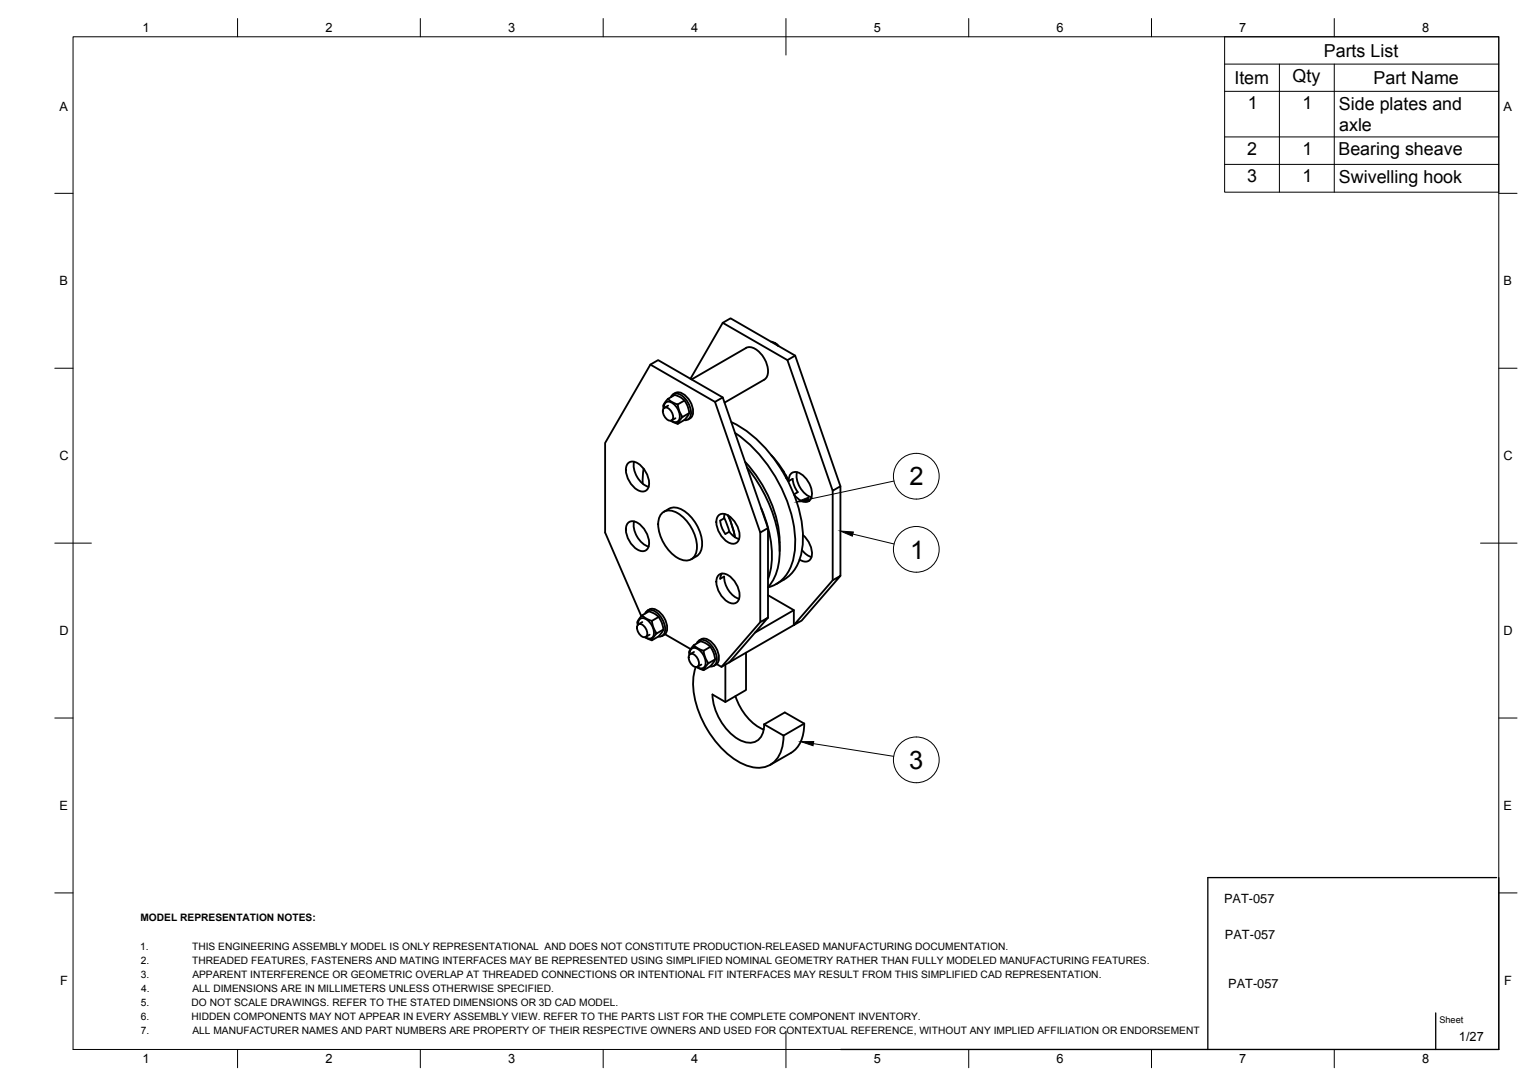
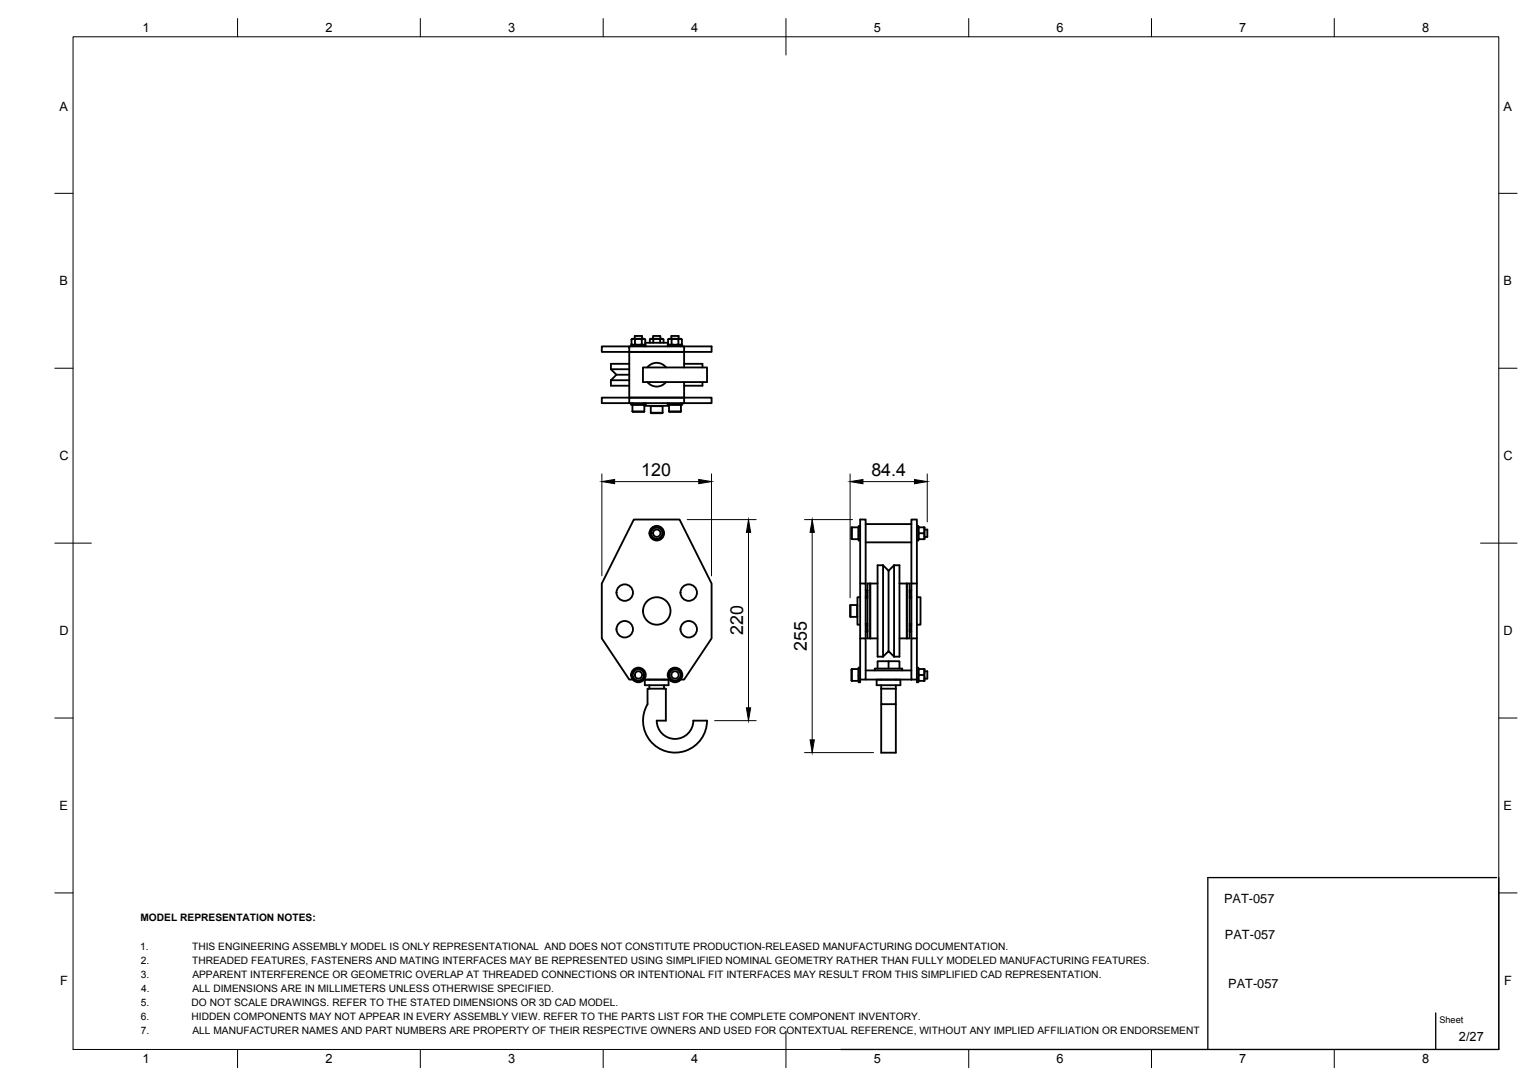
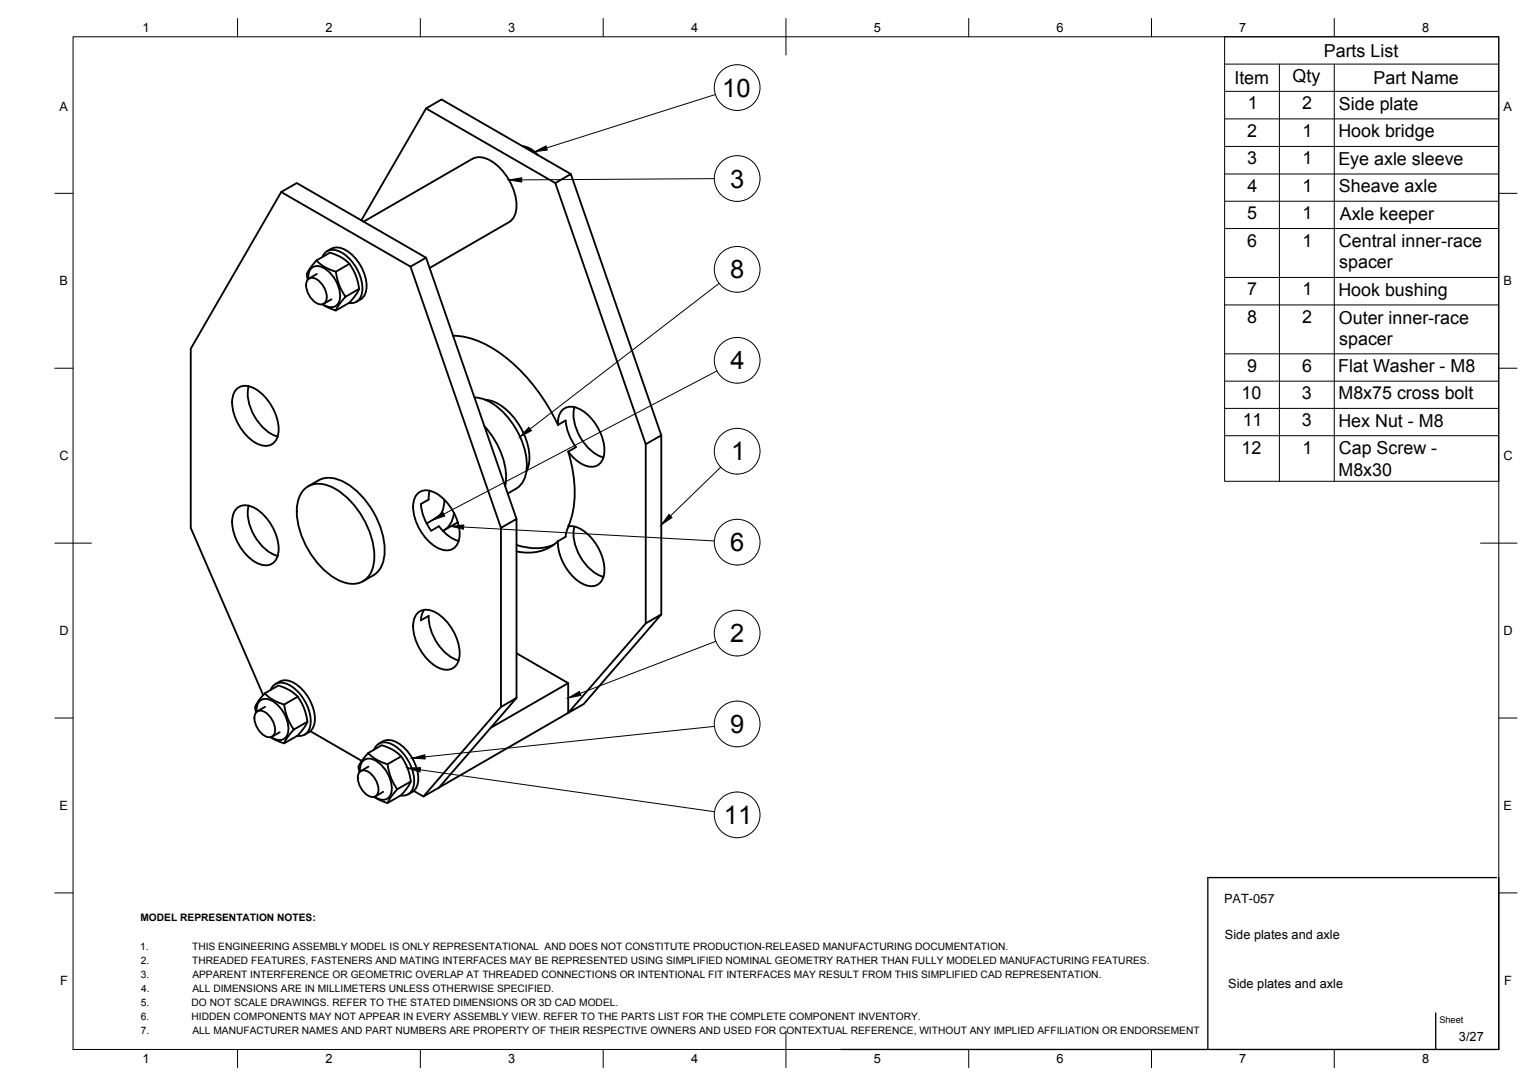
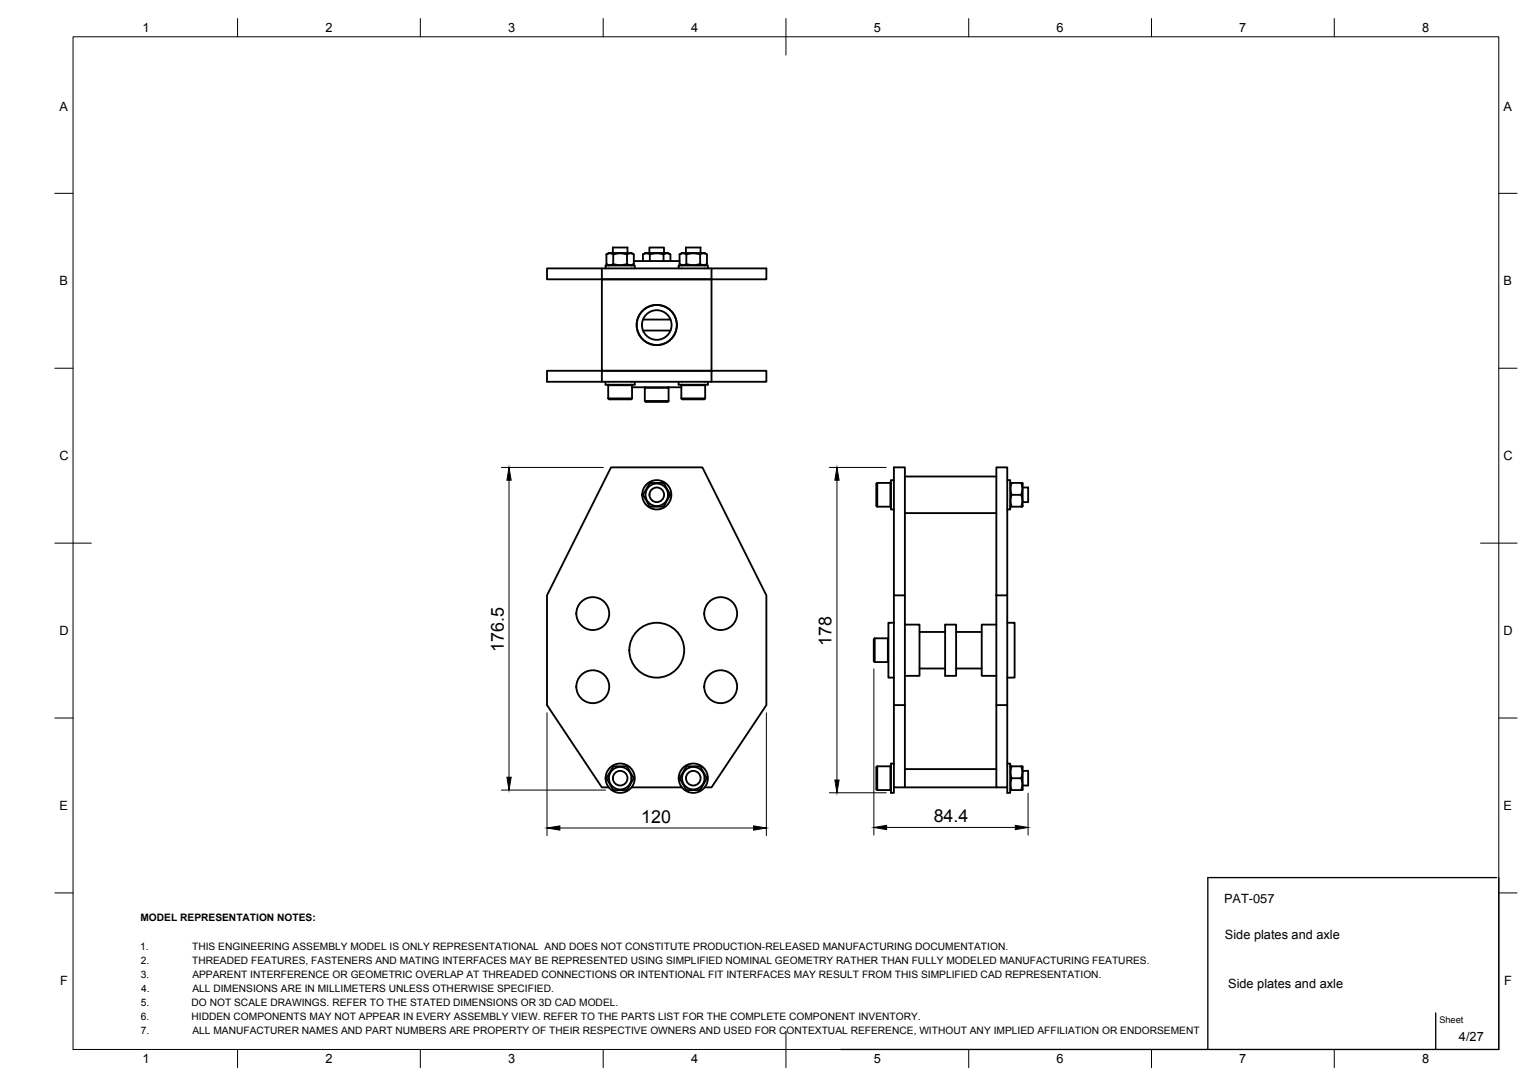
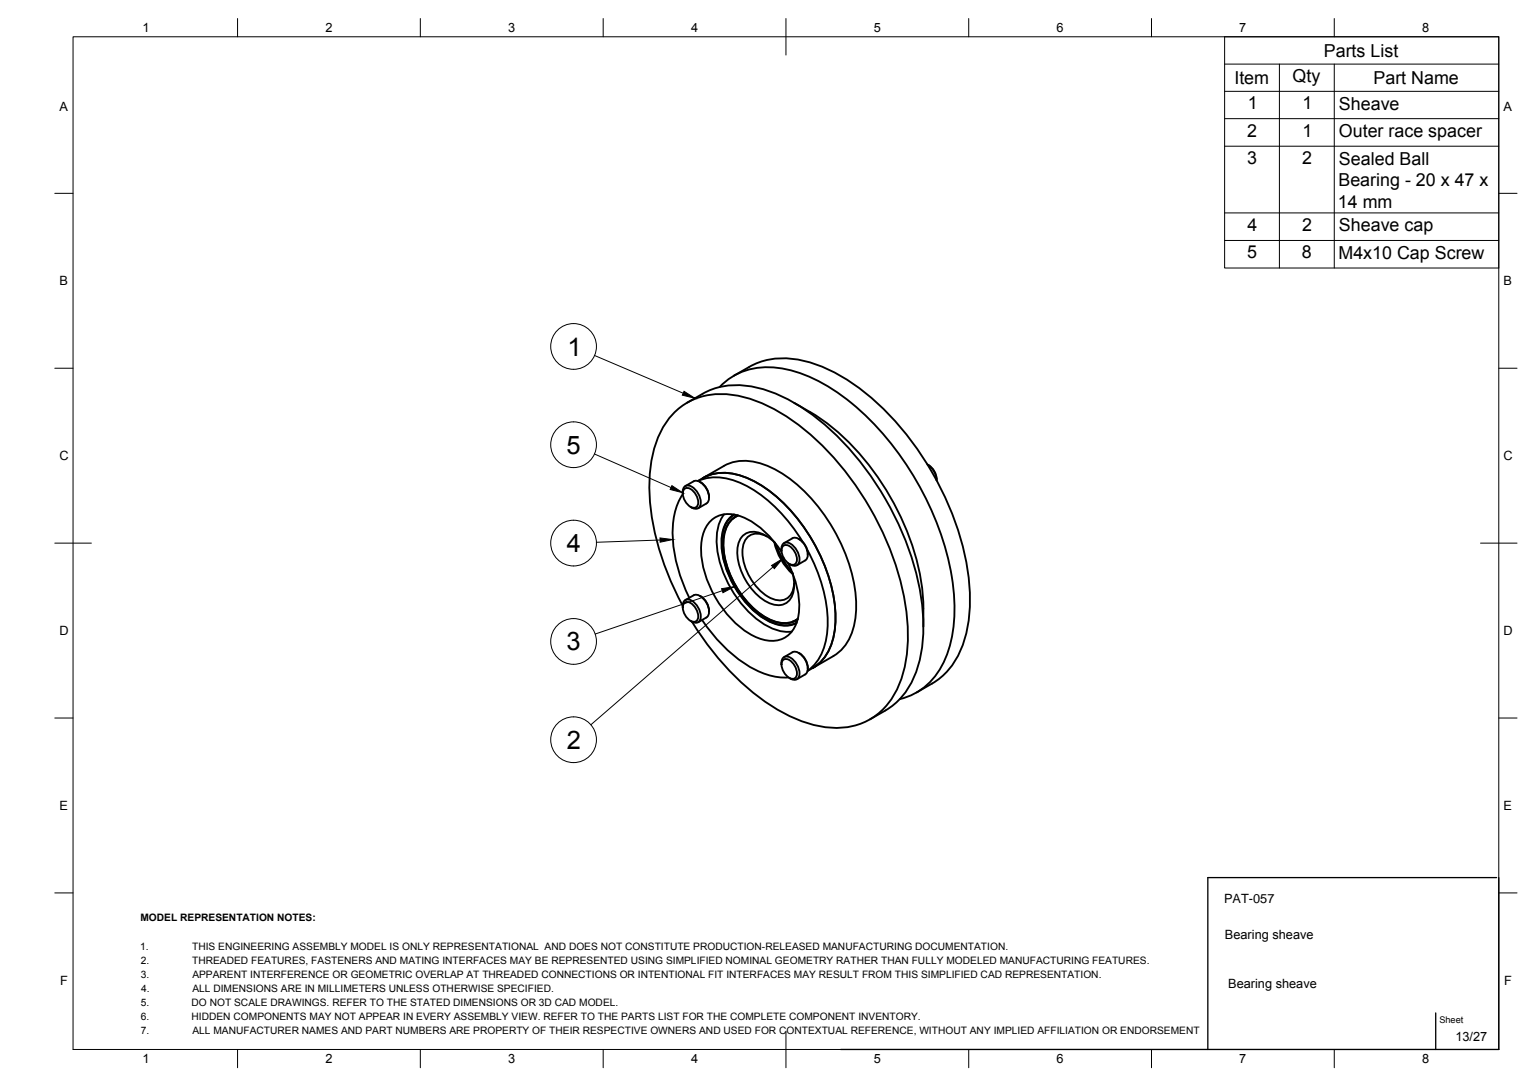
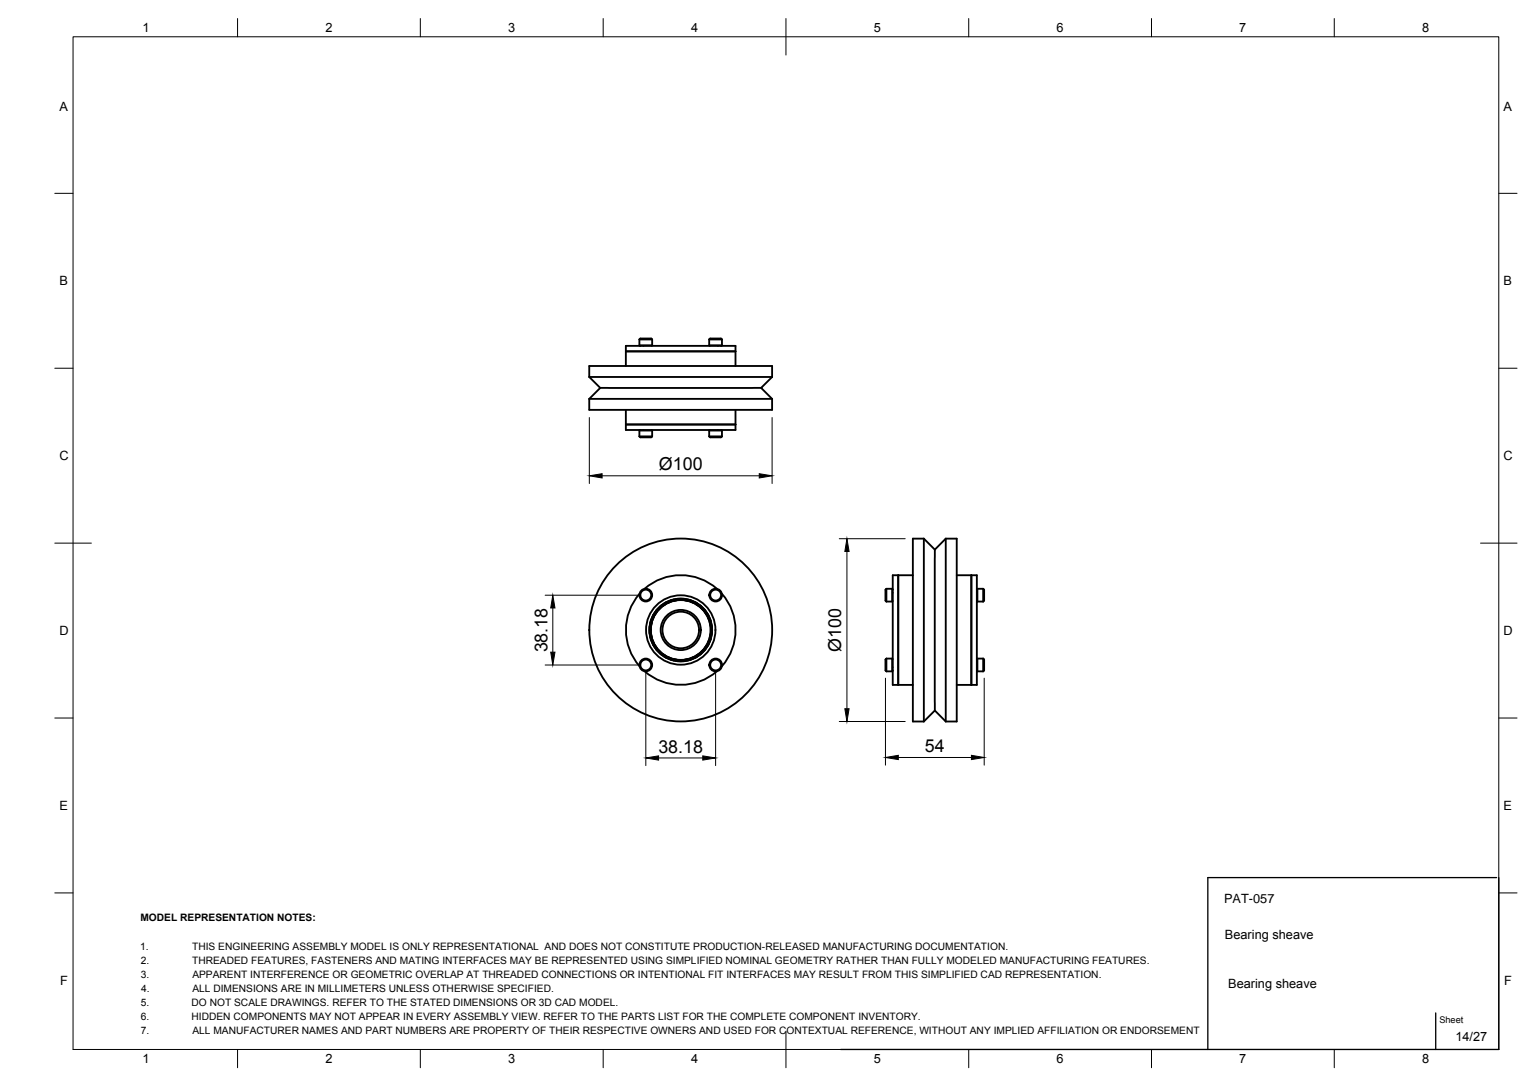
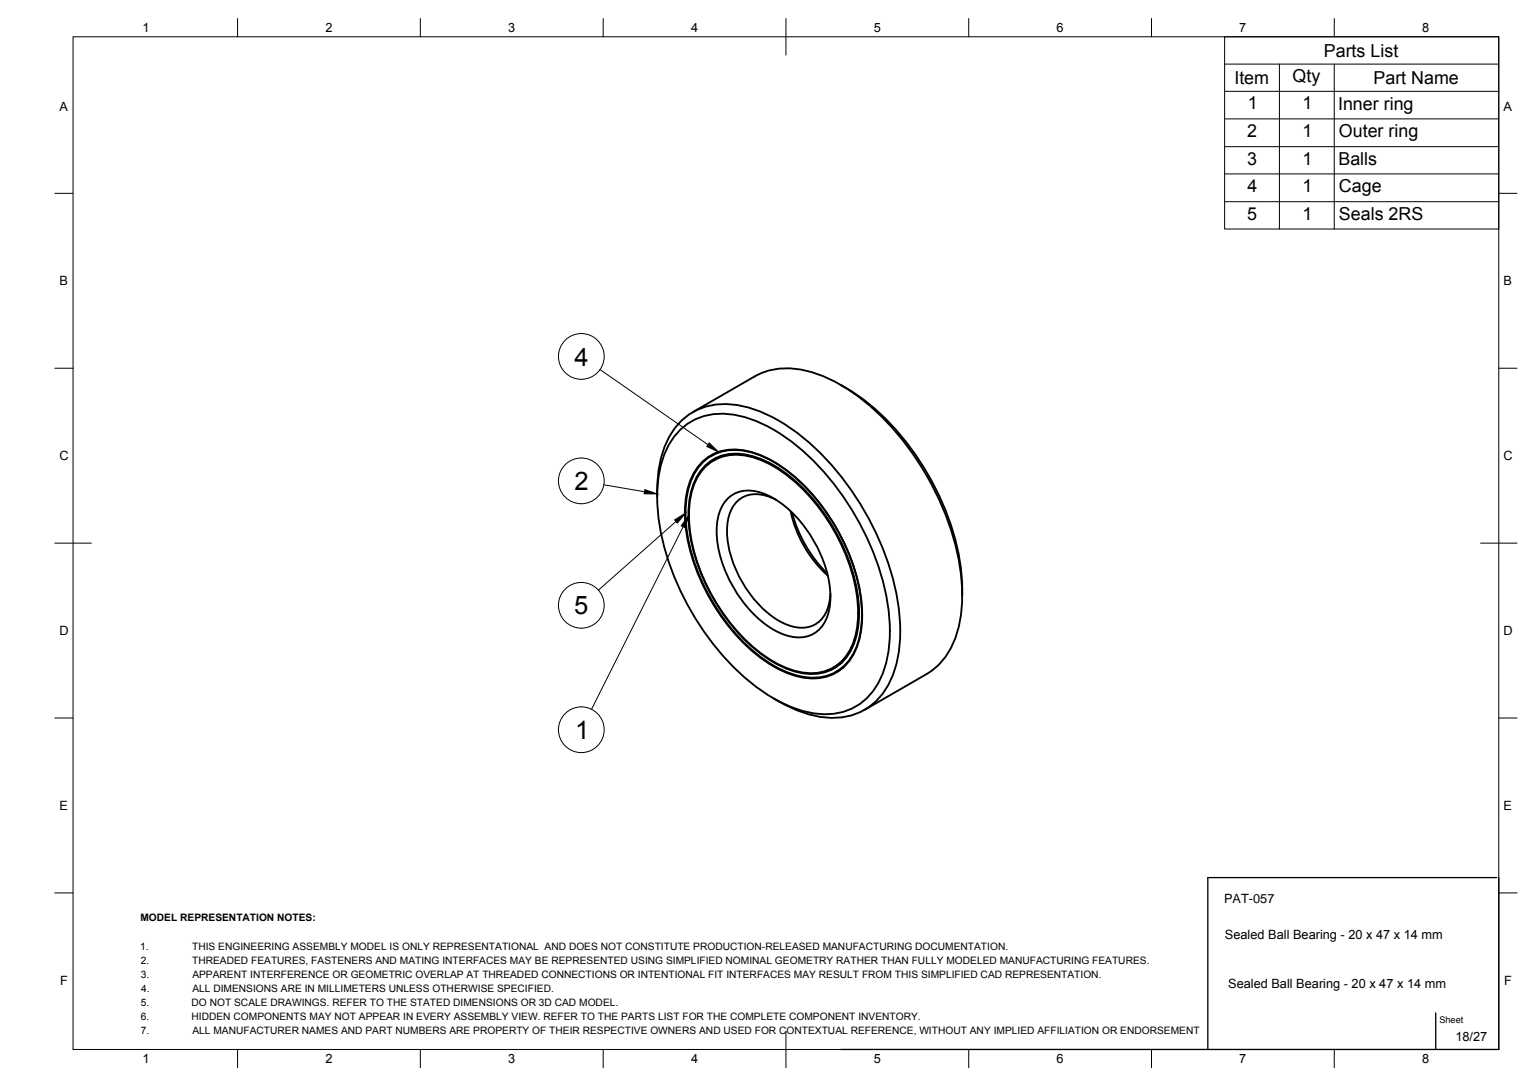
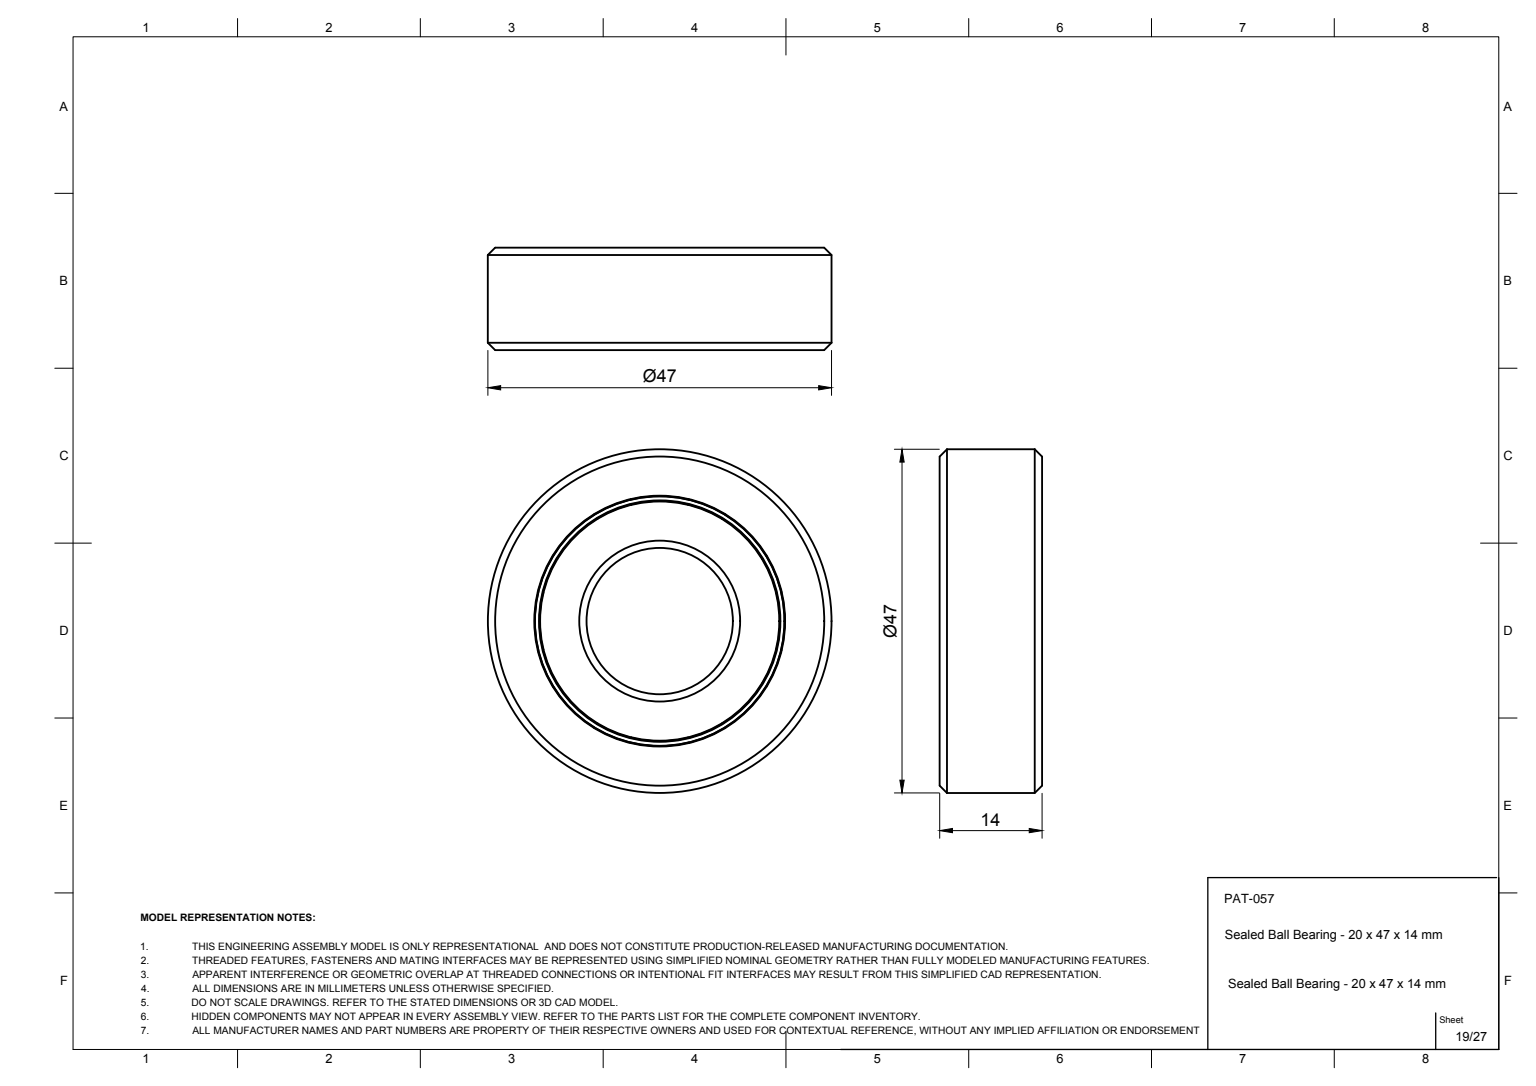
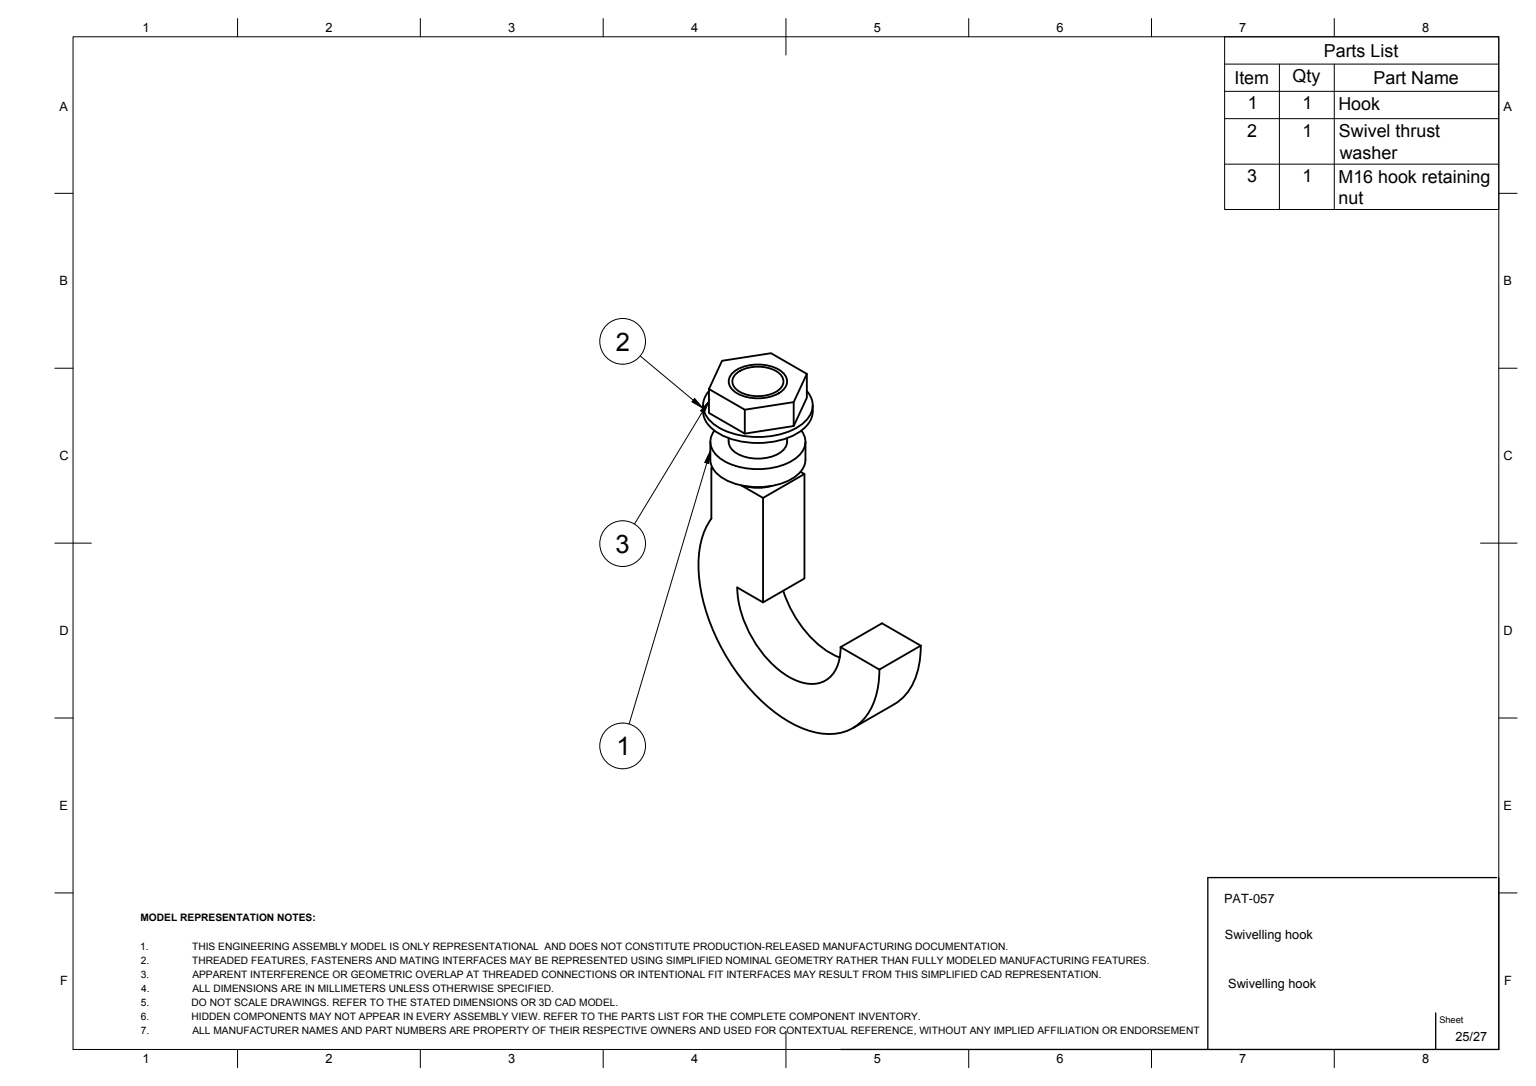
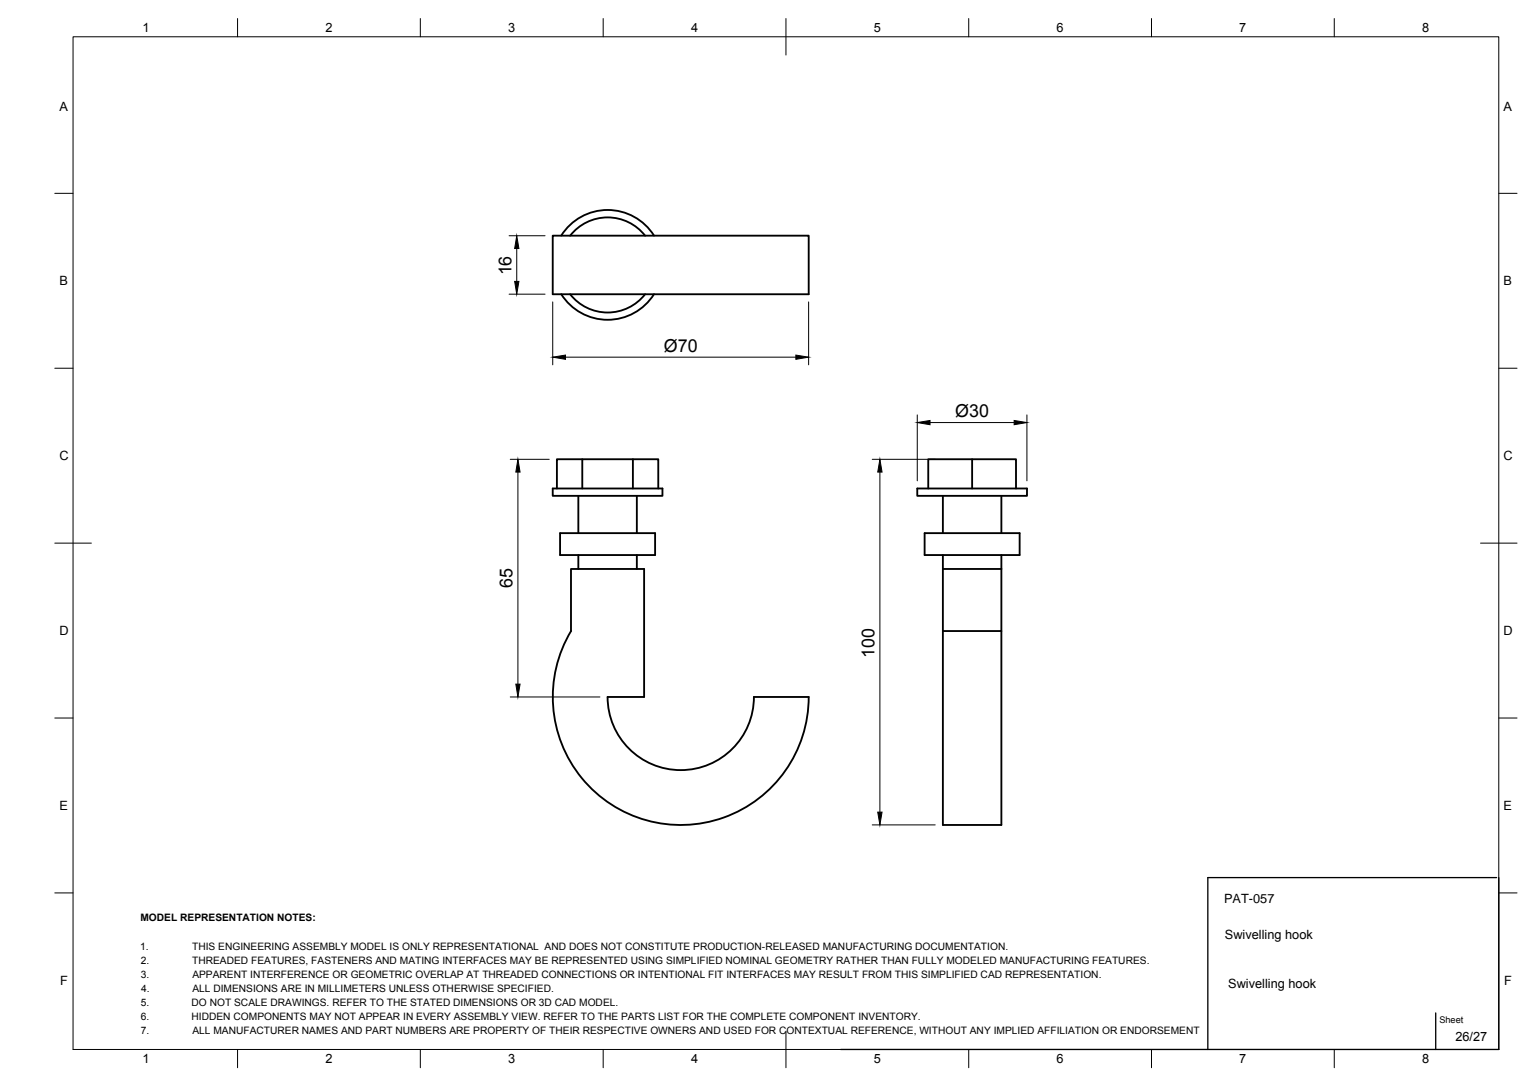
ISO-10303-21;
HEADER;
/* Generated by software containing ST-Developer
 * from STEP Tools, Inc. (www.steptools.com) 
 */

FILE_DESCRIPTION(
/* description */ ('Bearing-mounted hook block'),
/* implementation_level */ '2;1');

FILE_NAME(
/* name */ 'PAT-057',
/* time_stamp */ '2026-10-28T22:30:11-07:00',
/* author */ (''),
/* organization */ (''),
/* preprocessor_version */ 'ST-DEVELOPER v20.2',
/* originating_system */ 'Autodesk Translation Framework v15.17.0.0',
/* authorisation */ '');

FILE_SCHEMA (('AUTOMOTIVE_DESIGN { 1 0 10303 214 3 1 1 }'));
ENDSEC;

DATA;
#10=MECHANICAL_DESIGN_GEOMETRIC_PRESENTATION_REPRESENTATION('',(#323,#324,
#325,#326,#327,#328,#329,#330,#331,#332,#333,#334,#335,#336,#337,#338,#339,
#340,#341,#342,#343,#344,#345,#346,#347,#348,#349,#350,#351,#352,#353,#354),
#7609);
#11=B_SPLINE_CURVE_WITH_KNOTS('',3,(#6806,#6807,#6808,#6809,#6810,#6811,
#6812,#6813,#6814,#6815,#6816,#6817,#6818,#6819,#6820,#6821,#6822,#6823,
#6824,#6825,#6826,#6827),.UNSPECIFIED.,.F.,.F.,(4,2,2,2,2,2,2,2,2,2,4),
(0.0789094028588958,0.210573405340968,0.315860108011452,0.421146810681936,
0.522142632548711,0.623138454415485,0.72413427628226,0.825130098149035,
0.930416800819519,1.03570350349,1.16736750597208),.UNSPECIFIED.);
#12=B_SPLINE_CURVE_WITH_KNOTS('',3,(#6831,#6832,#6833,#6834,#6835,#6836,
#6837,#6838,#6839,#6840,#6841,#6842,#6843,#6844,#6845,#6846,#6847,#6848,
#6849,#6850,#6851,#6852),.UNSPECIFIED.,.F.,.F.,(4,2,2,2,2,2,2,2,2,2,4),
(0.0774793363974613,0.142088896491891,0.284177792983782,0.411119756996526,
0.514392970548519,0.617666184100513,0.720939397652506,0.8242126112045,0.951154575217244,
1.09324347170913,1.15785303180356),.UNSPECIFIED.);
#13=B_SPLINE_CURVE_WITH_KNOTS('',3,(#6858,#6859,#6860,#6861,#6862,#6863,
#6864,#6865,#6866,#6867,#6868,#6869,#6870,#6871,#6872,#6873,#6874,#6875,
#6876,#6877,#6878,#6879),.UNSPECIFIED.,.F.,.F.,(4,2,2,2,2,2,2,2,2,2,4),
(0.0774793363974613,0.142088896491891,0.284177792983782,0.411119756996525,
0.514392970548519,0.617666184100513,0.720939397652506,0.8242126112045,0.951154575217243,
1.09324347170913,1.15785303180356),.UNSPECIFIED.);
#14=B_SPLINE_CURVE_WITH_KNOTS('',3,(#6883,#6884,#6885,#6886,#6887,#6888,
#6889,#6890,#6891,#6892,#6893,#6894,#6895,#6896,#6897,#6898,#6899,#6900,
#6901,#6902,#6903,#6904),.UNSPECIFIED.,.F.,.F.,(4,2,2,2,2,2,2,2,2,2,4),
(0.0774793363974614,0.142088896491891,0.284177792983781,0.411119756996525,
0.514392970548519,0.617666184100512,0.720939397652506,0.824212611204499,
0.951154575217243,1.09324347170913,1.15785303180356),.UNSPECIFIED.);
#15=B_SPLINE_CURVE_WITH_KNOTS('',3,(#6908,#6909,#6910,#6911,#6912,#6913,
#6914,#6915,#6916,#6917,#6918,#6919),.UNSPECIFIED.,.F.,.F.,(4,2,2,2,2,4),
(0.0774793363974613,0.142088896491891,0.284177792983781,0.411119756996525,
0.514392970548519,0.617666184100512),.UNSPECIFIED.);
#16=B_SPLINE_CURVE_WITH_KNOTS('',3,(#6924,#6925,#6926,#6927,#6928,#6929,
#6930,#6931,#6932,#6933,#6934,#6935),.UNSPECIFIED.,.F.,.F.,(4,2,2,2,2,4),
(0.617666184100512,0.720939397652506,0.824212611204499,0.951154575217243,
1.09324347170913,1.15785303180356),.UNSPECIFIED.);
#17=B_SPLINE_CURVE_WITH_KNOTS('',3,(#6939,#6940,#6941,#6942,#6943,#6944,
#6945,#6946,#6947,#6948,#6949,#6950,#6951,#6952,#6953,#6954,#6955,#6956,
#6957,#6958,#6959,#6960),.UNSPECIFIED.,.F.,.F.,(4,2,2,2,2,2,2,2,2,2,4),
(0.0774793363974613,0.142088896491891,0.284177792983782,0.411119756996526,
0.514392970548519,0.617666184100513,0.720939397652507,0.8242126112045,0.951154575217245,
1.09324347170914,1.15785303180356),.UNSPECIFIED.);
#18=B_SPLINE_CURVE_WITH_KNOTS('',3,(#6964,#6965,#6966,#6967,#6968,#6969,
#6970,#6971,#6972,#6973,#6974,#6975,#6976,#6977,#6978,#6979,#6980,#6981,
#6982,#6983,#6984,#6985),.UNSPECIFIED.,.F.,.F.,(4,2,2,2,2,2,2,2,2,2,4),
(0.0774793363974613,0.142088896491891,0.284177792983782,0.411119756996526,
0.514392970548519,0.617666184100513,0.720939397652506,0.824212611204499,
0.951154575217243,1.09324347170913,1.15785303180356),.UNSPECIFIED.);
#19=B_SPLINE_CURVE_WITH_KNOTS('',3,(#6989,#6990,#6991,#6992,#6993,#6994,
#6995,#6996,#6997,#6998,#6999,#7000,#7001,#7002,#7003,#7004,#7005,#7006,
#7007,#7008,#7009,#7010),.UNSPECIFIED.,.F.,.F.,(4,2,2,2,2,2,2,2,2,2,4),
(0.0774793363974613,0.142088896491891,0.284177792983782,0.411119756996526,
0.514392970548519,0.617666184100513,0.720939397652506,0.8242126112045,0.951154575217244,
1.09324347170913,1.15785303180356),.UNSPECIFIED.);
#20=B_SPLINE_CURVE_WITH_KNOTS('',3,(#7014,#7015,#7016,#7017,#7018,#7019,
#7020,#7021,#7022,#7023,#7024,#7025,#7026,#7027,#7028,#7029,#7030,#7031,
#7032,#7033,#7034,#7035),.UNSPECIFIED.,.F.,.F.,(4,2,2,2,2,2,2,2,2,2,4),
(0.0774793363974613,0.142088896491891,0.284177792983782,0.411119756996526,
0.514392970548519,0.617666184100513,0.720939397652506,0.8242126112045,0.951154575217243,
1.09324347170913,1.15785303180356),.UNSPECIFIED.);
#21=B_SPLINE_CURVE_WITH_KNOTS('',3,(#7043,#7044,#7045,#7046,#7047,#7048,
#7049,#7050,#7051,#7052,#7053,#7054,#7055,#7056,#7057,#7058,#7059,#7060,
#7061,#7062,#7063,#7064),.UNSPECIFIED.,.F.,.F.,(4,2,2,2,2,2,2,2,2,2,4),
(0.0789094028588958,0.210573405340968,0.315860108011452,0.421146810681936,
0.522142632548711,0.623138454415485,0.72413427628226,0.825130098149035,
0.930416800819519,1.03570350349,1.16736750597208),.UNSPECIFIED.);
#22=B_SPLINE_CURVE_WITH_KNOTS('',3,(#7072,#7073,#7074,#7075,#7076,#7077,
#7078,#7079,#7080,#7081,#7082,#7083,#7084,#7085,#7086,#7087,#7088,#7089,
#7090,#7091,#7092,#7093),.UNSPECIFIED.,.F.,.F.,(4,2,2,2,2,2,2,2,2,2,4),
(0.0789094028588958,0.210573405340969,0.315860108011453,0.421146810681937,
0.522142632548712,0.623138454415486,0.724134276282261,0.825130098149035,
0.930416800819519,1.03570350349,1.16736750597208),.UNSPECIFIED.);
#23=B_SPLINE_CURVE_WITH_KNOTS('',3,(#7102,#7103,#7104,#7105,#7106,#7107,
#7108,#7109,#7110,#7111,#7112,#7113),.UNSPECIFIED.,.F.,.F.,(4,2,2,2,2,4),
(0.0789094028588958,0.210573405340968,0.315860108011452,0.421146810681937,
0.522142632548711,0.623138454415486),.UNSPECIFIED.);
#24=B_SPLINE_CURVE_WITH_KNOTS('',3,(#7115,#7116,#7117,#7118,#7119,#7120,
#7121,#7122,#7123,#7124,#7125,#7126),.UNSPECIFIED.,.F.,.F.,(4,2,2,2,2,4),
(0.623138454415486,0.72413427628226,0.825130098149035,0.930416800819519,
1.03570350349,1.16736750597208),.UNSPECIFIED.);
#25=B_SPLINE_CURVE_WITH_KNOTS('',3,(#7133,#7134,#7135,#7136,#7137,#7138,
#7139,#7140,#7141,#7142,#7143,#7144,#7145,#7146,#7147,#7148,#7149,#7150,
#7151,#7152,#7153,#7154),.UNSPECIFIED.,.F.,.F.,(4,2,2,2,2,2,2,2,2,2,4),
(0.0789094028588958,0.210573405340968,0.315860108011452,0.421146810681936,
0.522142632548711,0.623138454415486,0.72413427628226,0.825130098149035,
0.930416800819519,1.03570350349,1.16736750597208),.UNSPECIFIED.);
#26=B_SPLINE_CURVE_WITH_KNOTS('',3,(#7162,#7163,#7164,#7165,#7166,#7167,
#7168,#7169,#7170,#7171,#7172,#7173,#7174,#7175,#7176,#7177,#7178,#7179,
#7180,#7181,#7182,#7183),.UNSPECIFIED.,.F.,.F.,(4,2,2,2,2,2,2,2,2,2,4),
(0.0789094028588957,0.210573405340968,0.315860108011452,0.421146810681936,
0.522142632548711,0.623138454415485,0.72413427628226,0.825130098149035,
0.930416800819519,1.03570350349,1.16736750597207),.UNSPECIFIED.);
#27=B_SPLINE_CURVE_WITH_KNOTS('',3,(#7191,#7192,#7193,#7194,#7195,#7196,
#7197,#7198,#7199,#7200,#7201,#7202,#7203,#7204,#7205,#7206,#7207,#7208,
#7209,#7210,#7211,#7212),.UNSPECIFIED.,.F.,.F.,(4,2,2,2,2,2,2,2,2,2,4),
(0.0789094028588958,0.210573405340968,0.315860108011452,0.421146810681936,
0.522142632548711,0.623138454415486,0.72413427628226,0.825130098149035,
0.930416800819519,1.03570350349,1.16736750597208),.UNSPECIFIED.);
#28=B_SPLINE_CURVE_WITH_KNOTS('',3,(#7221,#7222,#7223,#7224,#7225,#7226,
#7227,#7228,#7229,#7230,#7231,#7232,#7233,#7234,#7235,#7236,#7237,#7238,
#7239,#7240,#7241,#7242),.UNSPECIFIED.,.F.,.F.,(4,2,2,2,2,2,2,2,2,2,4),
(0.0789094028588958,0.210573405340968,0.315860108011452,0.421146810681936,
0.522142632548711,0.623138454415485,0.72413427628226,0.825130098149035,
0.930416800819519,1.03570350349,1.16736750597208),.UNSPECIFIED.);
#29=SPHERICAL_SURFACE('',#4545,0.3969);
#30=SPHERICAL_SURFACE('',#4547,0.3969);
#31=SPHERICAL_SURFACE('',#4549,0.3969);
#32=SPHERICAL_SURFACE('',#4551,0.3969);
#33=SPHERICAL_SURFACE('',#4553,0.3969);
#34=SPHERICAL_SURFACE('',#4555,0.3969);
#35=SPHERICAL_SURFACE('',#4557,0.3969);
#36=SPHERICAL_SURFACE('',#4559,0.3969);
#37=SPHERICAL_SURFACE('',#4562,0.412776);
#38=SPHERICAL_SURFACE('',#4578,0.412776);
#39=SPHERICAL_SURFACE('',#4583,0.412776);
#40=SPHERICAL_SURFACE('',#4588,0.412776);
#41=SPHERICAL_SURFACE('',#4593,0.412776);
#42=SPHERICAL_SURFACE('',#4598,0.412776);
#43=SPHERICAL_SURFACE('',#4603,0.412776);
#44=SPHERICAL_SURFACE('',#4611,0.412776);
#45=TOROIDAL_SURFACE('',#4505,1.675,0.412776);
#46=TOROIDAL_SURFACE('',#4525,1.675,0.412776);
#47=ITEM_DEFINED_TRANSFORMATION($,$,#4221,#4435);
#48=ITEM_DEFINED_TRANSFORMATION($,$,#4221,#4436);
#49=ITEM_DEFINED_TRANSFORMATION($,$,#4281,#4437);
#50=ITEM_DEFINED_TRANSFORMATION($,$,#4297,#4438);
#51=ITEM_DEFINED_TRANSFORMATION($,$,#4306,#4439);
#52=ITEM_DEFINED_TRANSFORMATION($,$,#4320,#4440);
#53=ITEM_DEFINED_TRANSFORMATION($,$,#4329,#4441);
#54=ITEM_DEFINED_TRANSFORMATION($,$,#4338,#4442);
#55=ITEM_DEFINED_TRANSFORMATION($,$,#4347,#4443);
#56=ITEM_DEFINED_TRANSFORMATION($,$,#4347,#4444);
#57=ITEM_DEFINED_TRANSFORMATION($,$,#4384,#4445);
#58=ITEM_DEFINED_TRANSFORMATION($,$,#4356,#4446);
#59=ITEM_DEFINED_TRANSFORMATION($,$,#4384,#4447);
#60=ITEM_DEFINED_TRANSFORMATION($,$,#4393,#4448);
#61=ITEM_DEFINED_TRANSFORMATION($,$,#4384,#4449);
#62=ITEM_DEFINED_TRANSFORMATION($,$,#4356,#4450);
#63=ITEM_DEFINED_TRANSFORMATION($,$,#4384,#4451);
#64=ITEM_DEFINED_TRANSFORMATION($,$,#4393,#4452);
#65=ITEM_DEFINED_TRANSFORMATION($,$,#4384,#4453);
#66=ITEM_DEFINED_TRANSFORMATION($,$,#4356,#4454);
#67=ITEM_DEFINED_TRANSFORMATION($,$,#4384,#4455);
#68=ITEM_DEFINED_TRANSFORMATION($,$,#4393,#4456);
#69=ITEM_DEFINED_TRANSFORMATION($,$,#4409,#4457);
#70=ITEM_DEFINED_TRANSFORMATION($,$,#4504,#4632);
#71=ITEM_DEFINED_TRANSFORMATION($,$,#4524,#4633);
#72=ITEM_DEFINED_TRANSFORMATION($,$,#4544,#4634);
#73=ITEM_DEFINED_TRANSFORMATION($,$,#4561,#4635);
#74=ITEM_DEFINED_TRANSFORMATION($,$,#4615,#4636);
#75=ITEM_DEFINED_TRANSFORMATION($,$,#4459,#4686);
#76=ITEM_DEFINED_TRANSFORMATION($,$,#4494,#4687);
#77=ITEM_DEFINED_TRANSFORMATION($,$,#4503,#4688);
#78=ITEM_DEFINED_TRANSFORMATION($,$,#4503,#4689);
#79=ITEM_DEFINED_TRANSFORMATION($,$,#4637,#4690);
#80=ITEM_DEFINED_TRANSFORMATION($,$,#4637,#4691);
#81=ITEM_DEFINED_TRANSFORMATION($,$,#4662,#4692);
#82=ITEM_DEFINED_TRANSFORMATION($,$,#4662,#4693);
#83=ITEM_DEFINED_TRANSFORMATION($,$,#4662,#4694);
#84=ITEM_DEFINED_TRANSFORMATION($,$,#4662,#4695);
#85=ITEM_DEFINED_TRANSFORMATION($,$,#4662,#4696);
#86=ITEM_DEFINED_TRANSFORMATION($,$,#4662,#4697);
#87=ITEM_DEFINED_TRANSFORMATION($,$,#4662,#4698);
#88=ITEM_DEFINED_TRANSFORMATION($,$,#4662,#4699);
#89=ITEM_DEFINED_TRANSFORMATION($,$,#4701,#4751);
#90=ITEM_DEFINED_TRANSFORMATION($,$,#4730,#4752);
#91=ITEM_DEFINED_TRANSFORMATION($,$,#4739,#4753);
#92=ITEM_DEFINED_TRANSFORMATION($,$,#4220,#4754);
#93=ITEM_DEFINED_TRANSFORMATION($,$,#4458,#4755);
#94=ITEM_DEFINED_TRANSFORMATION($,$,#4700,#4756);
#95=(
REPRESENTATION_RELATIONSHIP($,$,#7722,#7721)
REPRESENTATION_RELATIONSHIP_WITH_TRANSFORMATION(#47)
SHAPE_REPRESENTATION_RELATIONSHIP()
);
#96=(
REPRESENTATION_RELATIONSHIP($,$,#7722,#7721)
REPRESENTATION_RELATIONSHIP_WITH_TRANSFORMATION(#48)
SHAPE_REPRESENTATION_RELATIONSHIP()
);
#97=(
REPRESENTATION_RELATIONSHIP($,$,#7723,#7721)
REPRESENTATION_RELATIONSHIP_WITH_TRANSFORMATION(#49)
SHAPE_REPRESENTATION_RELATIONSHIP()
);
#98=(
REPRESENTATION_RELATIONSHIP($,$,#7724,#7721)
REPRESENTATION_RELATIONSHIP_WITH_TRANSFORMATION(#50)
SHAPE_REPRESENTATION_RELATIONSHIP()
);
#99=(
REPRESENTATION_RELATIONSHIP($,$,#7725,#7721)
REPRESENTATION_RELATIONSHIP_WITH_TRANSFORMATION(#51)
SHAPE_REPRESENTATION_RELATIONSHIP()
);
#100=(
REPRESENTATION_RELATIONSHIP($,$,#7726,#7721)
REPRESENTATION_RELATIONSHIP_WITH_TRANSFORMATION(#52)
SHAPE_REPRESENTATION_RELATIONSHIP()
);
#101=(
REPRESENTATION_RELATIONSHIP($,$,#7727,#7721)
REPRESENTATION_RELATIONSHIP_WITH_TRANSFORMATION(#53)
SHAPE_REPRESENTATION_RELATIONSHIP()
);
#102=(
REPRESENTATION_RELATIONSHIP($,$,#7728,#7721)
REPRESENTATION_RELATIONSHIP_WITH_TRANSFORMATION(#54)
SHAPE_REPRESENTATION_RELATIONSHIP()
);
#103=(
REPRESENTATION_RELATIONSHIP($,$,#7729,#7721)
REPRESENTATION_RELATIONSHIP_WITH_TRANSFORMATION(#55)
SHAPE_REPRESENTATION_RELATIONSHIP()
);
#104=(
REPRESENTATION_RELATIONSHIP($,$,#7729,#7721)
REPRESENTATION_RELATIONSHIP_WITH_TRANSFORMATION(#56)
SHAPE_REPRESENTATION_RELATIONSHIP()
);
#105=(
REPRESENTATION_RELATIONSHIP($,$,#7731,#7721)
REPRESENTATION_RELATIONSHIP_WITH_TRANSFORMATION(#57)
SHAPE_REPRESENTATION_RELATIONSHIP()
);
#106=(
REPRESENTATION_RELATIONSHIP($,$,#7730,#7721)
REPRESENTATION_RELATIONSHIP_WITH_TRANSFORMATION(#58)
SHAPE_REPRESENTATION_RELATIONSHIP()
);
#107=(
REPRESENTATION_RELATIONSHIP($,$,#7731,#7721)
REPRESENTATION_RELATIONSHIP_WITH_TRANSFORMATION(#59)
SHAPE_REPRESENTATION_RELATIONSHIP()
);
#108=(
REPRESENTATION_RELATIONSHIP($,$,#7732,#7721)
REPRESENTATION_RELATIONSHIP_WITH_TRANSFORMATION(#60)
SHAPE_REPRESENTATION_RELATIONSHIP()
);
#109=(
REPRESENTATION_RELATIONSHIP($,$,#7731,#7721)
REPRESENTATION_RELATIONSHIP_WITH_TRANSFORMATION(#61)
SHAPE_REPRESENTATION_RELATIONSHIP()
);
#110=(
REPRESENTATION_RELATIONSHIP($,$,#7730,#7721)
REPRESENTATION_RELATIONSHIP_WITH_TRANSFORMATION(#62)
SHAPE_REPRESENTATION_RELATIONSHIP()
);
#111=(
REPRESENTATION_RELATIONSHIP($,$,#7731,#7721)
REPRESENTATION_RELATIONSHIP_WITH_TRANSFORMATION(#63)
SHAPE_REPRESENTATION_RELATIONSHIP()
);
#112=(
REPRESENTATION_RELATIONSHIP($,$,#7732,#7721)
REPRESENTATION_RELATIONSHIP_WITH_TRANSFORMATION(#64)
SHAPE_REPRESENTATION_RELATIONSHIP()
);
#113=(
REPRESENTATION_RELATIONSHIP($,$,#7731,#7721)
REPRESENTATION_RELATIONSHIP_WITH_TRANSFORMATION(#65)
SHAPE_REPRESENTATION_RELATIONSHIP()
);
#114=(
REPRESENTATION_RELATIONSHIP($,$,#7730,#7721)
REPRESENTATION_RELATIONSHIP_WITH_TRANSFORMATION(#66)
SHAPE_REPRESENTATION_RELATIONSHIP()
);
#115=(
REPRESENTATION_RELATIONSHIP($,$,#7731,#7721)
REPRESENTATION_RELATIONSHIP_WITH_TRANSFORMATION(#67)
SHAPE_REPRESENTATION_RELATIONSHIP()
);
#116=(
REPRESENTATION_RELATIONSHIP($,$,#7732,#7721)
REPRESENTATION_RELATIONSHIP_WITH_TRANSFORMATION(#68)
SHAPE_REPRESENTATION_RELATIONSHIP()
);
#117=(
REPRESENTATION_RELATIONSHIP($,$,#7733,#7721)
REPRESENTATION_RELATIONSHIP_WITH_TRANSFORMATION(#69)
SHAPE_REPRESENTATION_RELATIONSHIP()
);
#118=(
REPRESENTATION_RELATIONSHIP($,$,#7738,#7737)
REPRESENTATION_RELATIONSHIP_WITH_TRANSFORMATION(#70)
SHAPE_REPRESENTATION_RELATIONSHIP()
);
#119=(
REPRESENTATION_RELATIONSHIP($,$,#7739,#7737)
REPRESENTATION_RELATIONSHIP_WITH_TRANSFORMATION(#71)
SHAPE_REPRESENTATION_RELATIONSHIP()
);
#120=(
REPRESENTATION_RELATIONSHIP($,$,#7740,#7737)
REPRESENTATION_RELATIONSHIP_WITH_TRANSFORMATION(#72)
SHAPE_REPRESENTATION_RELATIONSHIP()
);
#121=(
REPRESENTATION_RELATIONSHIP($,$,#7741,#7737)
REPRESENTATION_RELATIONSHIP_WITH_TRANSFORMATION(#73)
SHAPE_REPRESENTATION_RELATIONSHIP()
);
#122=(
REPRESENTATION_RELATIONSHIP($,$,#7742,#7737)
REPRESENTATION_RELATIONSHIP_WITH_TRANSFORMATION(#74)
SHAPE_REPRESENTATION_RELATIONSHIP()
);
#123=(
REPRESENTATION_RELATIONSHIP($,$,#7735,#7734)
REPRESENTATION_RELATIONSHIP_WITH_TRANSFORMATION(#75)
SHAPE_REPRESENTATION_RELATIONSHIP()
);
#124=(
REPRESENTATION_RELATIONSHIP($,$,#7736,#7734)
REPRESENTATION_RELATIONSHIP_WITH_TRANSFORMATION(#76)
SHAPE_REPRESENTATION_RELATIONSHIP()
);
#125=(
REPRESENTATION_RELATIONSHIP($,$,#7737,#7734)
REPRESENTATION_RELATIONSHIP_WITH_TRANSFORMATION(#77)
SHAPE_REPRESENTATION_RELATIONSHIP()
);
#126=(
REPRESENTATION_RELATIONSHIP($,$,#7737,#7734)
REPRESENTATION_RELATIONSHIP_WITH_TRANSFORMATION(#78)
SHAPE_REPRESENTATION_RELATIONSHIP()
);
#127=(
REPRESENTATION_RELATIONSHIP($,$,#7743,#7734)
REPRESENTATION_RELATIONSHIP_WITH_TRANSFORMATION(#79)
SHAPE_REPRESENTATION_RELATIONSHIP()
);
#128=(
REPRESENTATION_RELATIONSHIP($,$,#7743,#7734)
REPRESENTATION_RELATIONSHIP_WITH_TRANSFORMATION(#80)
SHAPE_REPRESENTATION_RELATIONSHIP()
);
#129=(
REPRESENTATION_RELATIONSHIP($,$,#7744,#7734)
REPRESENTATION_RELATIONSHIP_WITH_TRANSFORMATION(#81)
SHAPE_REPRESENTATION_RELATIONSHIP()
);
#130=(
REPRESENTATION_RELATIONSHIP($,$,#7744,#7734)
REPRESENTATION_RELATIONSHIP_WITH_TRANSFORMATION(#82)
SHAPE_REPRESENTATION_RELATIONSHIP()
);
#131=(
REPRESENTATION_RELATIONSHIP($,$,#7744,#7734)
REPRESENTATION_RELATIONSHIP_WITH_TRANSFORMATION(#83)
SHAPE_REPRESENTATION_RELATIONSHIP()
);
#132=(
REPRESENTATION_RELATIONSHIP($,$,#7744,#7734)
REPRESENTATION_RELATIONSHIP_WITH_TRANSFORMATION(#84)
SHAPE_REPRESENTATION_RELATIONSHIP()
);
#133=(
REPRESENTATION_RELATIONSHIP($,$,#7744,#7734)
REPRESENTATION_RELATIONSHIP_WITH_TRANSFORMATION(#85)
SHAPE_REPRESENTATION_RELATIONSHIP()
);
#134=(
REPRESENTATION_RELATIONSHIP($,$,#7744,#7734)
REPRESENTATION_RELATIONSHIP_WITH_TRANSFORMATION(#86)
SHAPE_REPRESENTATION_RELATIONSHIP()
);
#135=(
REPRESENTATION_RELATIONSHIP($,$,#7744,#7734)
REPRESENTATION_RELATIONSHIP_WITH_TRANSFORMATION(#87)
SHAPE_REPRESENTATION_RELATIONSHIP()
);
#136=(
REPRESENTATION_RELATIONSHIP($,$,#7744,#7734)
REPRESENTATION_RELATIONSHIP_WITH_TRANSFORMATION(#88)
SHAPE_REPRESENTATION_RELATIONSHIP()
);
#137=(
REPRESENTATION_RELATIONSHIP($,$,#7746,#7745)
REPRESENTATION_RELATIONSHIP_WITH_TRANSFORMATION(#89)
SHAPE_REPRESENTATION_RELATIONSHIP()
);
#138=(
REPRESENTATION_RELATIONSHIP($,$,#7747,#7745)
REPRESENTATION_RELATIONSHIP_WITH_TRANSFORMATION(#90)
SHAPE_REPRESENTATION_RELATIONSHIP()
);
#139=(
REPRESENTATION_RELATIONSHIP($,$,#7748,#7745)
REPRESENTATION_RELATIONSHIP_WITH_TRANSFORMATION(#91)
SHAPE_REPRESENTATION_RELATIONSHIP()
);
#140=(
REPRESENTATION_RELATIONSHIP($,$,#7721,#7720)
REPRESENTATION_RELATIONSHIP_WITH_TRANSFORMATION(#92)
SHAPE_REPRESENTATION_RELATIONSHIP()
);
#141=(
REPRESENTATION_RELATIONSHIP($,$,#7734,#7720)
REPRESENTATION_RELATIONSHIP_WITH_TRANSFORMATION(#93)
SHAPE_REPRESENTATION_RELATIONSHIP()
);
#142=(
REPRESENTATION_RELATIONSHIP($,$,#7745,#7720)
REPRESENTATION_RELATIONSHIP_WITH_TRANSFORMATION(#94)
SHAPE_REPRESENTATION_RELATIONSHIP()
);
#143=CONTEXT_DEPENDENT_SHAPE_REPRESENTATION(#95,#7657);
#144=CONTEXT_DEPENDENT_SHAPE_REPRESENTATION(#96,#7658);
#145=CONTEXT_DEPENDENT_SHAPE_REPRESENTATION(#97,#7659);
#146=CONTEXT_DEPENDENT_SHAPE_REPRESENTATION(#98,#7660);
#147=CONTEXT_DEPENDENT_SHAPE_REPRESENTATION(#99,#7661);
#148=CONTEXT_DEPENDENT_SHAPE_REPRESENTATION(#100,#7662);
#149=CONTEXT_DEPENDENT_SHAPE_REPRESENTATION(#101,#7663);
#150=CONTEXT_DEPENDENT_SHAPE_REPRESENTATION(#102,#7664);
#151=CONTEXT_DEPENDENT_SHAPE_REPRESENTATION(#103,#7665);
#152=CONTEXT_DEPENDENT_SHAPE_REPRESENTATION(#104,#7666);
#153=CONTEXT_DEPENDENT_SHAPE_REPRESENTATION(#105,#7667);
#154=CONTEXT_DEPENDENT_SHAPE_REPRESENTATION(#106,#7668);
#155=CONTEXT_DEPENDENT_SHAPE_REPRESENTATION(#107,#7669);
#156=CONTEXT_DEPENDENT_SHAPE_REPRESENTATION(#108,#7670);
#157=CONTEXT_DEPENDENT_SHAPE_REPRESENTATION(#109,#7671);
#158=CONTEXT_DEPENDENT_SHAPE_REPRESENTATION(#110,#7672);
#159=CONTEXT_DEPENDENT_SHAPE_REPRESENTATION(#111,#7673);
#160=CONTEXT_DEPENDENT_SHAPE_REPRESENTATION(#112,#7674);
#161=CONTEXT_DEPENDENT_SHAPE_REPRESENTATION(#113,#7675);
#162=CONTEXT_DEPENDENT_SHAPE_REPRESENTATION(#114,#7676);
#163=CONTEXT_DEPENDENT_SHAPE_REPRESENTATION(#115,#7677);
#164=CONTEXT_DEPENDENT_SHAPE_REPRESENTATION(#116,#7678);
#165=CONTEXT_DEPENDENT_SHAPE_REPRESENTATION(#117,#7679);
#166=CONTEXT_DEPENDENT_SHAPE_REPRESENTATION(#118,#7689);
#167=CONTEXT_DEPENDENT_SHAPE_REPRESENTATION(#119,#7690);
#168=CONTEXT_DEPENDENT_SHAPE_REPRESENTATION(#120,#7691);
#169=CONTEXT_DEPENDENT_SHAPE_REPRESENTATION(#121,#7692);
#170=CONTEXT_DEPENDENT_SHAPE_REPRESENTATION(#122,#7693);
#171=CONTEXT_DEPENDENT_SHAPE_REPRESENTATION(#123,#7696);
#172=CONTEXT_DEPENDENT_SHAPE_REPRESENTATION(#124,#7697);
#173=CONTEXT_DEPENDENT_SHAPE_REPRESENTATION(#125,#7698);
#174=CONTEXT_DEPENDENT_SHAPE_REPRESENTATION(#126,#7699);
#175=CONTEXT_DEPENDENT_SHAPE_REPRESENTATION(#127,#7700);
#176=CONTEXT_DEPENDENT_SHAPE_REPRESENTATION(#128,#7701);
#177=CONTEXT_DEPENDENT_SHAPE_REPRESENTATION(#129,#7702);
#178=CONTEXT_DEPENDENT_SHAPE_REPRESENTATION(#130,#7703);
#179=CONTEXT_DEPENDENT_SHAPE_REPRESENTATION(#131,#7704);
#180=CONTEXT_DEPENDENT_SHAPE_REPRESENTATION(#132,#7705);
#181=CONTEXT_DEPENDENT_SHAPE_REPRESENTATION(#133,#7706);
#182=CONTEXT_DEPENDENT_SHAPE_REPRESENTATION(#134,#7707);
#183=CONTEXT_DEPENDENT_SHAPE_REPRESENTATION(#135,#7708);
#184=CONTEXT_DEPENDENT_SHAPE_REPRESENTATION(#136,#7709);
#185=CONTEXT_DEPENDENT_SHAPE_REPRESENTATION(#137,#7714);
#186=CONTEXT_DEPENDENT_SHAPE_REPRESENTATION(#138,#7715);
#187=CONTEXT_DEPENDENT_SHAPE_REPRESENTATION(#139,#7716);
#188=CONTEXT_DEPENDENT_SHAPE_REPRESENTATION(#140,#7717);
#189=CONTEXT_DEPENDENT_SHAPE_REPRESENTATION(#141,#7718);
#190=CONTEXT_DEPENDENT_SHAPE_REPRESENTATION(#142,#7719);
#191=NEXT_ASSEMBLY_USAGE_OCCURRENCE('Side plate:2','Side plate:2',
'Side plate:2',#7751,#7752,'Side plate:2');
#192=NEXT_ASSEMBLY_USAGE_OCCURRENCE('Side plate:3','Side plate:3',
'Side plate:3',#7751,#7752,'Side plate:3');
#193=NEXT_ASSEMBLY_USAGE_OCCURRENCE('Hook bridge:2','Hook bridge:2',
'Hook bridge:2',#7751,#7753,'Hook bridge:2');
#194=NEXT_ASSEMBLY_USAGE_OCCURRENCE('Eye axle sleeve:2',
'Eye axle sleeve:2','Eye axle sleeve:2',#7751,#7754,'Eye axle sleeve:2');
#195=NEXT_ASSEMBLY_USAGE_OCCURRENCE('Sheave axle:2','Sheave axle:2',
'Sheave axle:2',#7751,#7755,'Sheave axle:2');
#196=NEXT_ASSEMBLY_USAGE_OCCURRENCE('Axle keeper:2','Axle keeper:2',
'Axle keeper:2',#7751,#7756,'Axle keeper:2');
#197=NEXT_ASSEMBLY_USAGE_OCCURRENCE('Central inner-race spacer:2',
'Central inner-race spacer:2','Central inner-race spacer:2',#7751,#7757,
'Central inner-race spacer:2');
#198=NEXT_ASSEMBLY_USAGE_OCCURRENCE('Hook bushing:2','Hook bushing:2',
'Hook bushing:2',#7751,#7758,'Hook bushing:2');
#199=NEXT_ASSEMBLY_USAGE_OCCURRENCE('Outer inner-race spacer:2',
'Outer inner-race spacer:2','Outer inner-race spacer:2',#7751,#7759,
'Outer inner-race spacer:2');
#200=NEXT_ASSEMBLY_USAGE_OCCURRENCE('Outer inner-race spacer:3',
'Outer inner-race spacer:3','Outer inner-race spacer:3',#7751,#7759,
'Outer inner-race spacer:3');
#201=NEXT_ASSEMBLY_USAGE_OCCURRENCE('Flat Washer - M8:2',
'Flat Washer - M8:2','Flat Washer - M8:2',#7751,#7761,
'Flat Washer - M8:2');
#202=NEXT_ASSEMBLY_USAGE_OCCURRENCE('M8x75 cross bolt:2',
'M8x75 cross bolt:2','M8x75 cross bolt:2',#7751,#7760,
'M8x75 cross bolt:2');
#203=NEXT_ASSEMBLY_USAGE_OCCURRENCE('Flat Washer - M8:3',
'Flat Washer - M8:3','Flat Washer - M8:3',#7751,#7761,
'Flat Washer - M8:3');
#204=NEXT_ASSEMBLY_USAGE_OCCURRENCE('Hex Nut - M8:2','Hex Nut - M8:2',
'Hex Nut - M8:2',#7751,#7762,'Hex Nut - M8:2');
#205=NEXT_ASSEMBLY_USAGE_OCCURRENCE('Flat Washer - M8:4',
'Flat Washer - M8:4','Flat Washer - M8:4',#7751,#7761,
'Flat Washer - M8:4');
#206=NEXT_ASSEMBLY_USAGE_OCCURRENCE('M8x75 cross bolt:3',
'M8x75 cross bolt:3','M8x75 cross bolt:3',#7751,#7760,
'M8x75 cross bolt:3');
#207=NEXT_ASSEMBLY_USAGE_OCCURRENCE('Flat Washer - M8:5',
'Flat Washer - M8:5','Flat Washer - M8:5',#7751,#7761,
'Flat Washer - M8:5');
#208=NEXT_ASSEMBLY_USAGE_OCCURRENCE('Hex Nut - M8:3','Hex Nut - M8:3',
'Hex Nut - M8:3',#7751,#7762,'Hex Nut - M8:3');
#209=NEXT_ASSEMBLY_USAGE_OCCURRENCE('Flat Washer - M8:6',
'Flat Washer - M8:6','Flat Washer - M8:6',#7751,#7761,
'Flat Washer - M8:6');
#210=NEXT_ASSEMBLY_USAGE_OCCURRENCE('M8x75 cross bolt:4',
'M8x75 cross bolt:4','M8x75 cross bolt:4',#7751,#7760,
'M8x75 cross bolt:4');
#211=NEXT_ASSEMBLY_USAGE_OCCURRENCE('Flat Washer - M8:7',
'Flat Washer - M8:7','Flat Washer - M8:7',#7751,#7761,
'Flat Washer - M8:7');
#212=NEXT_ASSEMBLY_USAGE_OCCURRENCE('Hex Nut - M8:4','Hex Nut - M8:4',
'Hex Nut - M8:4',#7751,#7762,'Hex Nut - M8:4');
#213=NEXT_ASSEMBLY_USAGE_OCCURRENCE('Cap Screw - M8x30:2',
'Cap Screw - M8x30:2','Cap Screw - M8x30:2',#7751,#7763,
'Cap Screw - M8x30:2');
#214=NEXT_ASSEMBLY_USAGE_OCCURRENCE('Inner ring:1','Inner ring:1',
'Inner ring:1',#7767,#7768,'Inner ring:1');
#215=NEXT_ASSEMBLY_USAGE_OCCURRENCE('Outer ring:1','Outer ring:1',
'Outer ring:1',#7767,#7769,'Outer ring:1');
#216=NEXT_ASSEMBLY_USAGE_OCCURRENCE('Balls:1','Balls:1','Balls:1',#7767,
#7770,'Balls:1');
#217=NEXT_ASSEMBLY_USAGE_OCCURRENCE('Cage:1','Cage:1','Cage:1',#7767,#7771,
'Cage:1');
#218=NEXT_ASSEMBLY_USAGE_OCCURRENCE('Seals 2RS:1','Seals 2RS:1',
'Seals 2RS:1',#7767,#7772,'Seals 2RS:1');
#219=NEXT_ASSEMBLY_USAGE_OCCURRENCE('Sheave:2','Sheave:2','Sheave:2',#7764,
#7765,'Sheave:2');
#220=NEXT_ASSEMBLY_USAGE_OCCURRENCE('Outer race spacer:2',
'Outer race spacer:2','Outer race spacer:2',#7764,#7766,
'Outer race spacer:2');
#221=NEXT_ASSEMBLY_USAGE_OCCURRENCE(
'Sealed Ball Bearing - 20 x 47 x 14 mm:2',
'Sealed Ball Bearing - 20 x 47 x 14 mm:2',
'Sealed Ball Bearing - 20 x 47 x 14 mm:2',#7764,#7767,
'Sealed Ball Bearing - 20 x 47 x 14 mm:2');
#222=NEXT_ASSEMBLY_USAGE_OCCURRENCE(
'Sealed Ball Bearing - 20 x 47 x 14 mm:3',
'Sealed Ball Bearing - 20 x 47 x 14 mm:3',
'Sealed Ball Bearing - 20 x 47 x 14 mm:3',#7764,#7767,
'Sealed Ball Bearing - 20 x 47 x 14 mm:3');
#223=NEXT_ASSEMBLY_USAGE_OCCURRENCE('Sheave cap:2','Sheave cap:2',
'Sheave cap:2',#7764,#7773,'Sheave cap:2');
#224=NEXT_ASSEMBLY_USAGE_OCCURRENCE('Sheave cap:3','Sheave cap:3',
'Sheave cap:3',#7764,#7773,'Sheave cap:3');
#225=NEXT_ASSEMBLY_USAGE_OCCURRENCE('M4x10 Cap Screw:2',
'M4x10 Cap Screw:2','M4x10 Cap Screw:2',#7764,#7774,'M4x10 Cap Screw:2');
#226=NEXT_ASSEMBLY_USAGE_OCCURRENCE('M4x10 Cap Screw:3',
'M4x10 Cap Screw:3','M4x10 Cap Screw:3',#7764,#7774,'M4x10 Cap Screw:3');
#227=NEXT_ASSEMBLY_USAGE_OCCURRENCE('M4x10 Cap Screw:4',
'M4x10 Cap Screw:4','M4x10 Cap Screw:4',#7764,#7774,'M4x10 Cap Screw:4');
#228=NEXT_ASSEMBLY_USAGE_OCCURRENCE('M4x10 Cap Screw:5',
'M4x10 Cap Screw:5','M4x10 Cap Screw:5',#7764,#7774,'M4x10 Cap Screw:5');
#229=NEXT_ASSEMBLY_USAGE_OCCURRENCE('M4x10 Cap Screw:6',
'M4x10 Cap Screw:6','M4x10 Cap Screw:6',#7764,#7774,'M4x10 Cap Screw:6');
#230=NEXT_ASSEMBLY_USAGE_OCCURRENCE('M4x10 Cap Screw:7',
'M4x10 Cap Screw:7','M4x10 Cap Screw:7',#7764,#7774,'M4x10 Cap Screw:7');
#231=NEXT_ASSEMBLY_USAGE_OCCURRENCE('M4x10 Cap Screw:8',
'M4x10 Cap Screw:8','M4x10 Cap Screw:8',#7764,#7774,'M4x10 Cap Screw:8');
#232=NEXT_ASSEMBLY_USAGE_OCCURRENCE('M4x10 Cap Screw:9',
'M4x10 Cap Screw:9','M4x10 Cap Screw:9',#7764,#7774,'M4x10 Cap Screw:9');
#233=NEXT_ASSEMBLY_USAGE_OCCURRENCE('Hook:2','Hook:2','Hook:2',#7775,#7776,
'Hook:2');
#234=NEXT_ASSEMBLY_USAGE_OCCURRENCE('Swivel thrust washer:2',
'Swivel thrust washer:2','Swivel thrust washer:2',#7775,#7777,
'Swivel thrust washer:2');
#235=NEXT_ASSEMBLY_USAGE_OCCURRENCE('M16 hook retaining nut:2',
'M16 hook retaining nut:2','M16 hook retaining nut:2',#7775,#7778,
'M16 hook retaining nut:2');
#236=NEXT_ASSEMBLY_USAGE_OCCURRENCE('Side plates and axle:1',
'Side plates and axle:1','Side plates and axle:1',#7750,#7751,
'Side plates and axle:1');
#237=NEXT_ASSEMBLY_USAGE_OCCURRENCE('Bearing sheave:1',
'Bearing sheave:1','Bearing sheave:1',#7750,#7764,'Bearing sheave:1');
#238=NEXT_ASSEMBLY_USAGE_OCCURRENCE('Swivelling hook:1',
'Swivelling hook:1','Swivelling hook:1',#7750,#7775,'Swivelling hook:1');
#239=(
BOUNDED_CURVE()
B_SPLINE_CURVE(2,(#6451,#6452,#6453),.UNSPECIFIED.,.F.,.F.)
B_SPLINE_CURVE_WITH_KNOTS((3,3),(0.14973948338295,0.97160236658079),
 .UNSPECIFIED.)
CURVE()
GEOMETRIC_REPRESENTATION_ITEM()
RATIONAL_B_SPLINE_CURVE((1.07140024848292,1.23714644374248,1.07140024848292))
REPRESENTATION_ITEM('')
);
#240=(
BOUNDED_CURVE()
B_SPLINE_CURVE(2,(#6455,#6456,#6457),.UNSPECIFIED.,.F.,.F.)
B_SPLINE_CURVE_WITH_KNOTS((3,3),(0.14973948338295,0.971602366580789),
 .UNSPECIFIED.)
CURVE()
GEOMETRIC_REPRESENTATION_ITEM()
RATIONAL_B_SPLINE_CURVE((1.07140024848292,1.23714644374248,1.07140024848292))
REPRESENTATION_ITEM('')
);
#241=(
BOUNDED_CURVE()
B_SPLINE_CURVE(2,(#6462,#6463,#6464),.UNSPECIFIED.,.F.,.F.)
B_SPLINE_CURVE_WITH_KNOTS((3,3),(0.14973948338295,0.97160236658079),
 .UNSPECIFIED.)
CURVE()
GEOMETRIC_REPRESENTATION_ITEM()
RATIONAL_B_SPLINE_CURVE((1.07140024848292,1.23714644374248,1.07140024848292))
REPRESENTATION_ITEM('')
);
#242=(
BOUNDED_CURVE()
B_SPLINE_CURVE(2,(#6466,#6467,#6468),.UNSPECIFIED.,.F.,.F.)
B_SPLINE_CURVE_WITH_KNOTS((3,3),(0.14973948338295,0.97160236658079),
 .UNSPECIFIED.)
CURVE()
GEOMETRIC_REPRESENTATION_ITEM()
RATIONAL_B_SPLINE_CURVE((1.07140024848292,1.23714644374248,1.07140024848292))
REPRESENTATION_ITEM('')
);
#243=(
BOUNDED_CURVE()
B_SPLINE_CURVE(2,(#6470,#6471,#6472),.UNSPECIFIED.,.F.,.F.)
B_SPLINE_CURVE_WITH_KNOTS((3,3),(0.14973948338295,0.971602366580789),
 .UNSPECIFIED.)
CURVE()
GEOMETRIC_REPRESENTATION_ITEM()
RATIONAL_B_SPLINE_CURVE((1.07140024848292,1.23714644374248,1.07140024848292))
REPRESENTATION_ITEM('')
);
#244=(
BOUNDED_CURVE()
B_SPLINE_CURVE(2,(#6473,#6474,#6475),.UNSPECIFIED.,.F.,.F.)
B_SPLINE_CURVE_WITH_KNOTS((3,3),(0.14973948338295,0.97160236658079),
 .UNSPECIFIED.)
CURVE()
GEOMETRIC_REPRESENTATION_ITEM()
RATIONAL_B_SPLINE_CURVE((1.07140024848292,1.23714644374248,1.07140024848292))
REPRESENTATION_ITEM('')
);
#245=(
BOUNDED_CURVE()
B_SPLINE_CURVE(2,(#6482,#6483,#6484),.UNSPECIFIED.,.F.,.F.)
B_SPLINE_CURVE_WITH_KNOTS((3,3),(0.14973948338295,0.97160236658079),
 .UNSPECIFIED.)
CURVE()
GEOMETRIC_REPRESENTATION_ITEM()
RATIONAL_B_SPLINE_CURVE((1.07140024848292,1.23714644374248,1.07140024848292))
REPRESENTATION_ITEM('')
);
#246=(
BOUNDED_CURVE()
B_SPLINE_CURVE(2,(#6486,#6487,#6488),.UNSPECIFIED.,.F.,.F.)
B_SPLINE_CURVE_WITH_KNOTS((3,3),(0.14973948338295,0.97160236658079),
 .UNSPECIFIED.)
CURVE()
GEOMETRIC_REPRESENTATION_ITEM()
RATIONAL_B_SPLINE_CURVE((1.07140024848292,1.23714644374248,1.07140024848292))
REPRESENTATION_ITEM('')
);
#247=(
BOUNDED_CURVE()
B_SPLINE_CURVE(2,(#6490,#6491,#6492),.UNSPECIFIED.,.F.,.F.)
B_SPLINE_CURVE_WITH_KNOTS((3,3),(0.14973948338295,0.971602366580789),
 .UNSPECIFIED.)
CURVE()
GEOMETRIC_REPRESENTATION_ITEM()
RATIONAL_B_SPLINE_CURVE((1.07140024848292,1.23714644374248,1.07140024848292))
REPRESENTATION_ITEM('')
);
#248=(
BOUNDED_CURVE()
B_SPLINE_CURVE(2,(#6494,#6495,#6496),.UNSPECIFIED.,.F.,.F.)
B_SPLINE_CURVE_WITH_KNOTS((3,3),(0.14973948338295,0.97160236658079),
 .UNSPECIFIED.)
CURVE()
GEOMETRIC_REPRESENTATION_ITEM()
RATIONAL_B_SPLINE_CURVE((1.07140024848292,1.23714644374248,1.07140024848292))
REPRESENTATION_ITEM('')
);
#249=(
BOUNDED_CURVE()
B_SPLINE_CURVE(2,(#6498,#6499,#6500),.UNSPECIFIED.,.F.,.F.)
B_SPLINE_CURVE_WITH_KNOTS((3,3),(0.14973948338295,0.97160236658079),
 .UNSPECIFIED.)
CURVE()
GEOMETRIC_REPRESENTATION_ITEM()
RATIONAL_B_SPLINE_CURVE((1.07140024848292,1.23714644374248,1.07140024848292))
REPRESENTATION_ITEM('')
);
#250=(
BOUNDED_CURVE()
B_SPLINE_CURVE(2,(#6501,#6502,#6503),.UNSPECIFIED.,.F.,.F.)
B_SPLINE_CURVE_WITH_KNOTS((3,3),(0.14973948338295,0.971602366580789),
 .UNSPECIFIED.)
CURVE()
GEOMETRIC_REPRESENTATION_ITEM()
RATIONAL_B_SPLINE_CURVE((1.07140024848292,1.23714644374248,1.07140024848292))
REPRESENTATION_ITEM('')
);
#251=CONICAL_SURFACE('',#4373,0.625,0.785398163397448);
#252=CONICAL_SURFACE('',#4377,0.635,0.785398163397449);
#253=CONICAL_SURFACE('',#4381,0.41,0.463647609000806);
#254=CONICAL_SURFACE('',#4394,0.734027674973257,1.0471975511966);
#255=CONICAL_SURFACE('',#4396,0.734027674973257,1.0471975511966);
#256=CONICAL_SURFACE('',#4412,0.625,0.785398163397448);
#257=CONICAL_SURFACE('',#4416,0.635,0.785398163397449);
#258=CONICAL_SURFACE('',#4420,0.41,0.463647609000806);
#259=CONICAL_SURFACE('',#4424,0.36,0.785398163397448);
#260=CONICAL_SURFACE('',#4472,4.7,0.785398163397448);
#261=CONICAL_SURFACE('',#4475,4.7,0.785398163397448);
#262=CONICAL_SURFACE('',#4516,1.05,0.785398163397449);
#263=CONICAL_SURFACE('',#4523,1.05,0.785398163397449);
#264=CONICAL_SURFACE('',#4536,2.3,0.785398163397449);
#265=CONICAL_SURFACE('',#4540,2.3,0.785398163397449);
#266=CONICAL_SURFACE('',#4675,0.325,0.785398163397448);
#267=CONICAL_SURFACE('',#4679,0.335,0.785398163397448);
#268=CONICAL_SURFACE('',#4683,0.21,0.463647609000806);
#269=ORIENTED_CLOSED_SHELL('',*,#3927,.F.);
#270=ORIENTED_CLOSED_SHELL('',*,#3932,.F.);
#271=ORIENTED_CLOSED_SHELL('',*,#3949,.F.);
#272=BREP_WITH_VOIDS('Body1',#3928,(#269));
#273=BREP_WITH_VOIDS('Body1',#3931,(#270));
#274=BREP_WITH_VOIDS('Body1',#3950,(#271));
#275=SHAPE_REPRESENTATION_RELATIONSHIP('SRR','None',#7722,#299);
#276=SHAPE_REPRESENTATION_RELATIONSHIP('SRR','None',#7723,#300);
#277=SHAPE_REPRESENTATION_RELATIONSHIP('SRR','None',#7724,#301);
#278=SHAPE_REPRESENTATION_RELATIONSHIP('SRR','None',#7725,#302);
#279=SHAPE_REPRESENTATION_RELATIONSHIP('SRR','None',#7726,#303);
#280=SHAPE_REPRESENTATION_RELATIONSHIP('SRR','None',#7727,#304);
#281=SHAPE_REPRESENTATION_RELATIONSHIP('SRR','None',#7728,#305);
#282=SHAPE_REPRESENTATION_RELATIONSHIP('SRR','None',#7729,#306);
#283=SHAPE_REPRESENTATION_RELATIONSHIP('SRR','None',#7730,#307);
#284=SHAPE_REPRESENTATION_RELATIONSHIP('SRR','None',#7731,#308);
#285=SHAPE_REPRESENTATION_RELATIONSHIP('SRR','None',#7732,#309);
#286=SHAPE_REPRESENTATION_RELATIONSHIP('SRR','None',#7733,#310);
#287=SHAPE_REPRESENTATION_RELATIONSHIP('SRR','None',#7735,#311);
#288=SHAPE_REPRESENTATION_RELATIONSHIP('SRR','None',#7736,#312);
#289=SHAPE_REPRESENTATION_RELATIONSHIP('SRR','None',#7738,#313);
#290=SHAPE_REPRESENTATION_RELATIONSHIP('SRR','None',#7739,#314);
#291=SHAPE_REPRESENTATION_RELATIONSHIP('SRR','None',#7740,#315);
#292=SHAPE_REPRESENTATION_RELATIONSHIP('SRR','None',#7741,#316);
#293=SHAPE_REPRESENTATION_RELATIONSHIP('SRR','None',#7742,#317);
#294=SHAPE_REPRESENTATION_RELATIONSHIP('SRR','None',#7743,#318);
#295=SHAPE_REPRESENTATION_RELATIONSHIP('SRR','None',#7744,#319);
#296=SHAPE_REPRESENTATION_RELATIONSHIP('SRR','None',#7746,#320);
#297=SHAPE_REPRESENTATION_RELATIONSHIP('SRR','None',#7747,#321);
#298=SHAPE_REPRESENTATION_RELATIONSHIP('SRR','None',#7748,#322);
#299=ADVANCED_BREP_SHAPE_REPRESENTATION('',(#355),#7582);
#300=ADVANCED_BREP_SHAPE_REPRESENTATION('',(#356),#7583);
#301=ADVANCED_BREP_SHAPE_REPRESENTATION('',(#357),#7584);
#302=ADVANCED_BREP_SHAPE_REPRESENTATION('',(#358),#7585);
#303=ADVANCED_BREP_SHAPE_REPRESENTATION('',(#359),#7586);
#304=ADVANCED_BREP_SHAPE_REPRESENTATION('',(#360),#7587);
#305=ADVANCED_BREP_SHAPE_REPRESENTATION('',(#361),#7588);
#306=ADVANCED_BREP_SHAPE_REPRESENTATION('',(#362),#7589);
#307=ADVANCED_BREP_SHAPE_REPRESENTATION('',(#272),#7590);
#308=ADVANCED_BREP_SHAPE_REPRESENTATION('',(#363),#7591);
#309=ADVANCED_BREP_SHAPE_REPRESENTATION('',(#364),#7592);
#310=ADVANCED_BREP_SHAPE_REPRESENTATION('',(#273),#7593);
#311=ADVANCED_BREP_SHAPE_REPRESENTATION('',(#365),#7595);
#312=ADVANCED_BREP_SHAPE_REPRESENTATION('',(#366),#7596);
#313=ADVANCED_BREP_SHAPE_REPRESENTATION('',(#367),#7598);
#314=ADVANCED_BREP_SHAPE_REPRESENTATION('',(#368),#7599);
#315=ADVANCED_BREP_SHAPE_REPRESENTATION('',(#369,#370,#371,#372,#373,#374,
#375,#376),#7600);
#316=ADVANCED_BREP_SHAPE_REPRESENTATION('',(#377),#7601);
#317=ADVANCED_BREP_SHAPE_REPRESENTATION('',(#378,#379),#7602);
#318=ADVANCED_BREP_SHAPE_REPRESENTATION('',(#380),#7603);
#319=ADVANCED_BREP_SHAPE_REPRESENTATION('',(#274),#7604);
#320=ADVANCED_BREP_SHAPE_REPRESENTATION('',(#381),#7606);
#321=ADVANCED_BREP_SHAPE_REPRESENTATION('',(#382),#7607);
#322=ADVANCED_BREP_SHAPE_REPRESENTATION('',(#383),#7608);
#323=STYLED_ITEM('',(#7924),#355);
#324=STYLED_ITEM('',(#7945),#356);
#325=STYLED_ITEM('',(#7931),#357);
#326=STYLED_ITEM('',(#7931),#358);
#327=STYLED_ITEM('',(#7931),#359);
#328=STYLED_ITEM('',(#7917),#360);
#329=STYLED_ITEM('',(#7917),#361);
#330=STYLED_ITEM('',(#7917),#362);
#331=STYLED_ITEM('',(#7938),#272);
#332=STYLED_ITEM('',(#7938),#363);
#333=STYLED_ITEM('',(#7938),#364);
#334=STYLED_ITEM('',(#7938),#273);
#335=STYLED_ITEM('',(#7924),#365);
#336=STYLED_ITEM('',(#7931),#366);
#337=STYLED_ITEM('',(#7931),#367);
#338=STYLED_ITEM('',(#7931),#368);
#339=STYLED_ITEM('',(#7931),#369);
#340=STYLED_ITEM('',(#7931),#370);
#341=STYLED_ITEM('',(#7931),#371);
#342=STYLED_ITEM('',(#7931),#372);
#343=STYLED_ITEM('',(#7931),#373);
#344=STYLED_ITEM('',(#7931),#374);
#345=STYLED_ITEM('',(#7931),#375);
#346=STYLED_ITEM('',(#7931),#376);
#347=STYLED_ITEM('',(#7931),#377);
#348=STYLED_ITEM('',(#7931),#378);
#349=STYLED_ITEM('',(#7931),#379);
#350=STYLED_ITEM('',(#7945),#380);
#351=STYLED_ITEM('',(#7938),#274);
#352=STYLED_ITEM('',(#7917),#381);
#353=STYLED_ITEM('',(#7938),#382);
#354=STYLED_ITEM('',(#7938),#383);
#355=MANIFOLD_SOLID_BREP('Body1',#3919);
#356=MANIFOLD_SOLID_BREP('Body1',#3920);
#357=MANIFOLD_SOLID_BREP('Body1',#3921);
#358=MANIFOLD_SOLID_BREP('Body1',#3922);
#359=MANIFOLD_SOLID_BREP('Body1',#3923);
#360=MANIFOLD_SOLID_BREP('Body1',#3924);
#361=MANIFOLD_SOLID_BREP('Body1',#3925);
#362=MANIFOLD_SOLID_BREP('Body1',#3926);
#363=MANIFOLD_SOLID_BREP('Body1',#3929);
#364=MANIFOLD_SOLID_BREP('Body1',#3930);
#365=MANIFOLD_SOLID_BREP('Body1',#3933);
#366=MANIFOLD_SOLID_BREP('Body1',#3934);
#367=MANIFOLD_SOLID_BREP('Body1',#3935);
#368=MANIFOLD_SOLID_BREP('Body1',#3936);
#369=MANIFOLD_SOLID_BREP('Body1',#3937);
#370=MANIFOLD_SOLID_BREP('Body2',#3938);
#371=MANIFOLD_SOLID_BREP('Body3',#3939);
#372=MANIFOLD_SOLID_BREP('Body4',#3940);
#373=MANIFOLD_SOLID_BREP('Body5',#3941);
#374=MANIFOLD_SOLID_BREP('Body6',#3942);
#375=MANIFOLD_SOLID_BREP('Body7',#3943);
#376=MANIFOLD_SOLID_BREP('Body8',#3944);
#377=MANIFOLD_SOLID_BREP('Continuous crown cage',#3945);
#378=MANIFOLD_SOLID_BREP('Body1',#3946);
#379=MANIFOLD_SOLID_BREP('Body2',#3947);
#380=MANIFOLD_SOLID_BREP('Body1',#3948);
#381=MANIFOLD_SOLID_BREP('Body1',#3951);
#382=MANIFOLD_SOLID_BREP('Body1',#3952);
#383=MANIFOLD_SOLID_BREP('Body1',#3953);
#384=LINE('',#6087,#614);
#385=LINE('',#6089,#615);
#386=LINE('',#6093,#616);
#387=LINE('',#6096,#617);
#388=LINE('',#6099,#618);
#389=LINE('',#6101,#619);
#390=LINE('',#6105,#620);
#391=LINE('',#6109,#621);
#392=LINE('',#6112,#622);
#393=LINE('',#6117,#623);
#394=LINE('',#6124,#624);
#395=LINE('',#6131,#625);
#396=LINE('',#6141,#626);
#397=LINE('',#6148,#627);
#398=LINE('',#6154,#628);
#399=LINE('',#6160,#629);
#400=LINE('',#6165,#630);
#401=LINE('',#6169,#631);
#402=LINE('',#6171,#632);
#403=LINE('',#6173,#633);
#404=LINE('',#6174,#634);
#405=LINE('',#6177,#635);
#406=LINE('',#6179,#636);
#407=LINE('',#6180,#637);
#408=LINE('',#6183,#638);
#409=LINE('',#6185,#639);
#410=LINE('',#6186,#640);
#411=LINE('',#6189,#641);
#412=LINE('',#6191,#642);
#413=LINE('',#6192,#643);
#414=LINE('',#6195,#644);
#415=LINE('',#6197,#645);
#416=LINE('',#6198,#646);
#417=LINE('',#6201,#647);
#418=LINE('',#6203,#648);
#419=LINE('',#6204,#649);
#420=LINE('',#6207,#650);
#421=LINE('',#6209,#651);
#422=LINE('',#6210,#652);
#423=LINE('',#6212,#653);
#424=LINE('',#6213,#654);
#425=LINE('',#6221,#655);
#426=LINE('',#6227,#656);
#427=LINE('',#6233,#657);
#428=LINE('',#6238,#658);
#429=LINE('',#6240,#659);
#430=LINE('',#6242,#660);
#431=LINE('',#6243,#661);
#432=LINE('',#6246,#662);
#433=LINE('',#6248,#663);
#434=LINE('',#6249,#664);
#435=LINE('',#6252,#665);
#436=LINE('',#6254,#666);
#437=LINE('',#6255,#667);
#438=LINE('',#6257,#668);
#439=LINE('',#6258,#669);
#440=LINE('',#6266,#670);
#441=LINE('',#6272,#671);
#442=LINE('',#6281,#672);
#443=LINE('',#6291,#673);
#444=LINE('',#6297,#674);
#445=LINE('',#6304,#675);
#446=LINE('',#6310,#676);
#447=LINE('',#6319,#677);
#448=LINE('',#6325,#678);
#449=LINE('',#6334,#679);
#450=LINE('',#6340,#680);
#451=LINE('',#6349,#681);
#452=LINE('',#6355,#682);
#453=LINE('',#6363,#683);
#454=LINE('',#6365,#684);
#455=LINE('',#6367,#685);
#456=LINE('',#6368,#686);
#457=LINE('',#6371,#687);
#458=LINE('',#6373,#688);
#459=LINE('',#6374,#689);
#460=LINE('',#6377,#690);
#461=LINE('',#6379,#691);
#462=LINE('',#6380,#692);
#463=LINE('',#6383,#693);
#464=LINE('',#6385,#694);
#465=LINE('',#6386,#695);
#466=LINE('',#6389,#696);
#467=LINE('',#6391,#697);
#468=LINE('',#6392,#698);
#469=LINE('',#6394,#699);
#470=LINE('',#6395,#700);
#471=LINE('',#6405,#701);
#472=LINE('',#6414,#702);
#473=LINE('',#6418,#703);
#474=LINE('',#6422,#704);
#475=LINE('',#6429,#705);
#476=LINE('',#6431,#706);
#477=LINE('',#6437,#707);
#478=LINE('',#6443,#708);
#479=LINE('',#6459,#709);
#480=LINE('',#6480,#710);
#481=LINE('',#6505,#711);
#482=LINE('',#6506,#712);
#483=LINE('',#6508,#713);
#484=LINE('',#6510,#714);
#485=LINE('',#6515,#715);
#486=LINE('',#6518,#716);
#487=LINE('',#6520,#717);
#488=LINE('',#6531,#718);
#489=LINE('',#6535,#719);
#490=LINE('',#6539,#720);
#491=LINE('',#6546,#721);
#492=LINE('',#6550,#722);
#493=LINE('',#6554,#723);
#494=LINE('',#6559,#724);
#495=LINE('',#6561,#725);
#496=LINE('',#6563,#726);
#497=LINE('',#6564,#727);
#498=LINE('',#6567,#728);
#499=LINE('',#6569,#729);
#500=LINE('',#6570,#730);
#501=LINE('',#6573,#731);
#502=LINE('',#6575,#732);
#503=LINE('',#6576,#733);
#504=LINE('',#6579,#734);
#505=LINE('',#6581,#735);
#506=LINE('',#6582,#736);
#507=LINE('',#6585,#737);
#508=LINE('',#6587,#738);
#509=LINE('',#6588,#739);
#510=LINE('',#6590,#740);
#511=LINE('',#6591,#741);
#512=LINE('',#6623,#742);
#513=LINE('',#6629,#743);
#514=LINE('',#6635,#744);
#515=LINE('',#6641,#745);
#516=LINE('',#6647,#746);
#517=LINE('',#6652,#747);
#518=LINE('',#6656,#748);
#519=LINE('',#6666,#749);
#520=LINE('',#6669,#750);
#521=LINE('',#6675,#751);
#522=LINE('',#6680,#752);
#523=LINE('',#6688,#753);
#524=LINE('',#6694,#754);
#525=LINE('',#6712,#755);
#526=LINE('',#6718,#756);
#527=LINE('',#6722,#757);
#528=LINE('',#6728,#758);
#529=LINE('',#6733,#759);
#530=LINE('',#6748,#760);
#531=LINE('',#6757,#761);
#532=LINE('',#6761,#762);
#533=LINE('',#6765,#763);
#534=LINE('',#6768,#764);
#535=LINE('',#6921,#765);
#536=LINE('',#7217,#766);
#537=LINE('',#7259,#767);
#538=LINE('',#7264,#768);
#539=LINE('',#7273,#769);
#540=LINE('',#7278,#770);
#541=LINE('',#7289,#771);
#542=LINE('',#7295,#772);
#543=LINE('',#7301,#773);
#544=LINE('',#7307,#774);
#545=LINE('',#7313,#775);
#546=LINE('',#7320,#776);
#547=LINE('',#7326,#777);
#548=LINE('',#7334,#778);
#549=LINE('',#7336,#779);
#550=LINE('',#7338,#780);
#551=LINE('',#7339,#781);
#552=LINE('',#7342,#782);
#553=LINE('',#7344,#783);
#554=LINE('',#7345,#784);
#555=LINE('',#7348,#785);
#556=LINE('',#7350,#786);
#557=LINE('',#7351,#787);
#558=LINE('',#7354,#788);
#559=LINE('',#7356,#789);
#560=LINE('',#7357,#790);
#561=LINE('',#7360,#791);
#562=LINE('',#7362,#792);
#563=LINE('',#7363,#793);
#564=LINE('',#7365,#794);
#565=LINE('',#7366,#795);
#566=LINE('',#7378,#796);
#567=LINE('',#7382,#797);
#568=LINE('',#7386,#798);
#569=LINE('',#7393,#799);
#570=LINE('',#7395,#800);
#571=LINE('',#7423,#801);
#572=LINE('',#7426,#802);
#573=LINE('',#7435,#803);
#574=LINE('',#7439,#804);
#575=LINE('',#7441,#805);
#576=LINE('',#7442,#806);
#577=LINE('',#7445,#807);
#578=LINE('',#7447,#808);
#579=LINE('',#7448,#809);
#580=LINE('',#7452,#810);
#581=LINE('',#7453,#811);
#582=LINE('',#7454,#812);
#583=LINE('',#7458,#813);
#584=LINE('',#7460,#814);
#585=LINE('',#7462,#815);
#586=LINE('',#7463,#816);
#587=LINE('',#7465,#817);
#588=LINE('',#7469,#818);
#589=LINE('',#7474,#819);
#590=LINE('',#7476,#820);
#591=LINE('',#7479,#821);
#592=LINE('',#7482,#822);
#593=LINE('',#7489,#823);
#594=LINE('',#7495,#824);
#595=LINE('',#7504,#825);
#596=LINE('',#7509,#826);
#597=LINE('',#7511,#827);
#598=LINE('',#7513,#828);
#599=LINE('',#7514,#829);
#600=LINE('',#7517,#830);
#601=LINE('',#7519,#831);
#602=LINE('',#7520,#832);
#603=LINE('',#7523,#833);
#604=LINE('',#7525,#834);
#605=LINE('',#7526,#835);
#606=LINE('',#7529,#836);
#607=LINE('',#7531,#837);
#608=LINE('',#7532,#838);
#609=LINE('',#7535,#839);
#610=LINE('',#7537,#840);
#611=LINE('',#7538,#841);
#612=LINE('',#7540,#842);
#613=LINE('',#7541,#843);
#614=VECTOR('',#4785,1.);
#615=VECTOR('',#4786,1.);
#616=VECTOR('',#4791,1.);
#617=VECTOR('',#4794,1.);
#618=VECTOR('',#4797,1.);
#619=VECTOR('',#4798,1.);
#620=VECTOR('',#4803,1.2);
#621=VECTOR('',#4808,1.);
#622=VECTOR('',#4811,1.);
#623=VECTOR('',#4816,0.9);
#624=VECTOR('',#4825,0.9);
#625=VECTOR('',#4834,0.9);
#626=VECTOR('',#4847,0.9);
#627=VECTOR('',#4856,0.425);
#628=VECTOR('',#4863,0.425);
#629=VECTOR('',#4870,0.425);
#630=VECTOR('',#4877,1.);
#631=VECTOR('',#4880,1.);
#632=VECTOR('',#4881,1.);
#633=VECTOR('',#4882,1.);
#634=VECTOR('',#4883,1.);
#635=VECTOR('',#4886,1.);
#636=VECTOR('',#4887,1.);
#637=VECTOR('',#4888,1.);
#638=VECTOR('',#4891,1.);
#639=VECTOR('',#4892,1.);
#640=VECTOR('',#4893,1.);
#641=VECTOR('',#4896,1.);
#642=VECTOR('',#4897,1.);
#643=VECTOR('',#4898,1.);
#644=VECTOR('',#4901,1.);
#645=VECTOR('',#4902,1.);
#646=VECTOR('',#4903,1.);
#647=VECTOR('',#4906,1.);
#648=VECTOR('',#4907,1.);
#649=VECTOR('',#4908,1.);
#650=VECTOR('',#4911,1.);
#651=VECTOR('',#4912,1.);
#652=VECTOR('',#4913,1.);
#653=VECTOR('',#4916,1.);
#654=VECTOR('',#4917,1.);
#655=VECTOR('',#4928,1.1);
#656=VECTOR('',#4935,0.425);
#657=VECTOR('',#4942,0.425);
#658=VECTOR('',#4947,1.);
#659=VECTOR('',#4948,1.);
#660=VECTOR('',#4949,1.);
#661=VECTOR('',#4950,1.);
#662=VECTOR('',#4953,1.);
#663=VECTOR('',#4954,1.);
#664=VECTOR('',#4955,1.);
#665=VECTOR('',#4958,1.);
#666=VECTOR('',#4959,1.);
#667=VECTOR('',#4960,1.);
#668=VECTOR('',#4963,1.);
#669=VECTOR('',#4964,1.);
#670=VECTOR('',#4975,0.425);
#671=VECTOR('',#4982,1.);
#672=VECTOR('',#4995,0.34);
#673=VECTOR('',#5008,1.5);
#674=VECTOR('',#5017,1.);
#675=VECTOR('',#5026,0.425);
#676=VECTOR('',#5033,1.5);
#677=VECTOR('',#5046,1.005);
#678=VECTOR('',#5053,1.4);
#679=VECTOR('',#5066,0.81);
#680=VECTOR('',#5073,1.1);
#681=VECTOR('',#5086,1.005);
#682=VECTOR('',#5093,1.4);
#683=VECTOR('',#5104,1.);
#684=VECTOR('',#5105,1.);
#685=VECTOR('',#5106,1.);
#686=VECTOR('',#5107,1.);
#687=VECTOR('',#5110,1.);
#688=VECTOR('',#5111,1.);
#689=VECTOR('',#5112,1.);
#690=VECTOR('',#5115,1.);
#691=VECTOR('',#5116,1.);
#692=VECTOR('',#5117,1.);
#693=VECTOR('',#5120,1.);
#694=VECTOR('',#5121,1.);
#695=VECTOR('',#5122,1.);
#696=VECTOR('',#5125,1.);
#697=VECTOR('',#5126,1.);
#698=VECTOR('',#5127,1.);
#699=VECTOR('',#5130,1.);
#700=VECTOR('',#5131,1.);
#701=VECTOR('',#5144,0.4);
#702=VECTOR('',#5157,0.625);
#703=VECTOR('',#5162,0.65);
#704=VECTOR('',#5167,0.635);
#705=VECTOR('',#5176,0.41);
#706=VECTOR('',#5179,0.4);
#707=VECTOR('',#5186,0.42);
#708=VECTOR('',#5193,0.8);
#709=VECTOR('',#5204,0.734027674973257);
#710=VECTOR('',#5211,0.734027674973257);
#711=VECTOR('',#5214,1.);
#712=VECTOR('',#5215,1.);
#713=VECTOR('',#5218,1.);
#714=VECTOR('',#5221,1.);
#715=VECTOR('',#5226,0.4);
#716=VECTOR('',#5231,1.);
#717=VECTOR('',#5234,1.);
#718=VECTOR('',#5251,0.625);
#719=VECTOR('',#5256,0.65);
#720=VECTOR('',#5261,0.635);
#721=VECTOR('',#5270,0.41);
#722=VECTOR('',#5275,0.4);
#723=VECTOR('',#5280,0.36);
#724=VECTOR('',#5285,1.);
#725=VECTOR('',#5286,1.);
#726=VECTOR('',#5287,1.);
#727=VECTOR('',#5288,1.);
#728=VECTOR('',#5291,1.);
#729=VECTOR('',#5292,1.);
#730=VECTOR('',#5293,1.);
#731=VECTOR('',#5296,1.);
#732=VECTOR('',#5297,1.);
#733=VECTOR('',#5298,1.);
#734=VECTOR('',#5301,1.);
#735=VECTOR('',#5302,1.);
#736=VECTOR('',#5303,1.);
#737=VECTOR('',#5306,1.);
#738=VECTOR('',#5307,1.);
#739=VECTOR('',#5308,1.);
#740=VECTOR('',#5311,1.);
#741=VECTOR('',#5312,1.);
#742=VECTOR('',#5371,0.165);
#743=VECTOR('',#5378,0.165);
#744=VECTOR('',#5385,0.165);
#745=VECTOR('',#5392,0.165);
#746=VECTOR('',#5399,4.7);
#747=VECTOR('',#5406,4.7);
#748=VECTOR('',#5411,5.);
#749=VECTOR('',#5424,5.);
#750=VECTOR('',#5427,3.);
#751=VECTOR('',#5434,2.35);
#752=VECTOR('',#5441,3.);
#753=VECTOR('',#5452,1.9);
#754=VECTOR('',#5459,2.34);
#755=VECTOR('',#5484,1.63531);
#756=VECTOR('',#5491,1.);
#757=VECTOR('',#5496,1.05);
#758=VECTOR('',#5505,1.63531);
#759=VECTOR('',#5512,1.05);
#760=VECTOR('',#5531,1.71469);
#761=VECTOR('',#5542,2.3);
#762=VECTOR('',#5547,2.35);
#763=VECTOR('',#5552,2.3);
#764=VECTOR('',#5557,1.71469);
#765=VECTOR('',#5608,1.706752);
#766=VECTOR('',#5685,1.643248);
#767=VECTOR('',#5714,1.70469);
#768=VECTOR('',#5721,1.65031);
#769=VECTOR('',#5732,1.70469);
#770=VECTOR('',#5739,1.65031);
#771=VECTOR('',#5756,0.225);
#772=VECTOR('',#5763,0.225);
#773=VECTOR('',#5770,0.225);
#774=VECTOR('',#5777,0.225);
#775=VECTOR('',#5784,2.34);
#776=VECTOR('',#5793,1.9);
#777=VECTOR('',#5800,3.);
#778=VECTOR('',#5811,1.);
#779=VECTOR('',#5812,1.);
#780=VECTOR('',#5813,1.);
#781=VECTOR('',#5814,1.);
#782=VECTOR('',#5817,1.);
#783=VECTOR('',#5818,1.);
#784=VECTOR('',#5819,1.);
#785=VECTOR('',#5822,1.);
#786=VECTOR('',#5823,1.);
#787=VECTOR('',#5824,1.);
#788=VECTOR('',#5827,1.);
#789=VECTOR('',#5828,1.);
#790=VECTOR('',#5829,1.);
#791=VECTOR('',#5832,1.);
#792=VECTOR('',#5833,1.);
#793=VECTOR('',#5834,1.);
#794=VECTOR('',#5837,1.);
#795=VECTOR('',#5838,1.);
#796=VECTOR('',#5855,0.325);
#797=VECTOR('',#5860,0.35);
#798=VECTOR('',#5865,0.335);
#799=VECTOR('',#5874,0.21);
#800=VECTOR('',#5877,0.2);
#801=VECTOR('',#5924,1.3);
#802=VECTOR('',#5927,0.8);
#803=VECTOR('',#5938,0.8);
#804=VECTOR('',#5943,1.);
#805=VECTOR('',#5944,1.);
#806=VECTOR('',#5945,1.);
#807=VECTOR('',#5948,1.);
#808=VECTOR('',#5949,1.);
#809=VECTOR('',#5950,1.);
#810=VECTOR('',#5953,1.);
#811=VECTOR('',#5954,1.);
#812=VECTOR('',#5955,1.);
#813=VECTOR('',#5958,1.);
#814=VECTOR('',#5959,1.);
#815=VECTOR('',#5960,1.);
#816=VECTOR('',#5961,1.);
#817=VECTOR('',#5964,1.);
#818=VECTOR('',#5967,1.);
#819=VECTOR('',#5974,1.);
#820=VECTOR('',#5977,1.);
#821=VECTOR('',#5980,1.);
#822=VECTOR('',#5985,1.);
#823=VECTOR('',#5994,0.81);
#824=VECTOR('',#6001,1.5);
#825=VECTOR('',#6014,0.7);
#826=VECTOR('',#6019,1.);
#827=VECTOR('',#6020,1.);
#828=VECTOR('',#6021,1.);
#829=VECTOR('',#6022,1.);
#830=VECTOR('',#6025,1.);
#831=VECTOR('',#6026,1.);
#832=VECTOR('',#6027,1.);
#833=VECTOR('',#6030,1.);
#834=VECTOR('',#6031,1.);
#835=VECTOR('',#6032,1.);
#836=VECTOR('',#6035,1.);
#837=VECTOR('',#6036,1.);
#838=VECTOR('',#6037,1.);
#839=VECTOR('',#6040,1.);
#840=VECTOR('',#6041,1.);
#841=VECTOR('',#6042,1.);
#842=VECTOR('',#6045,1.);
#843=VECTOR('',#6046,1.);
#844=CYLINDRICAL_SURFACE('',#4232,3.25);
#845=CYLINDRICAL_SURFACE('',#4234,3.25);
#846=CYLINDRICAL_SURFACE('',#4236,3.25);
#847=CYLINDRICAL_SURFACE('',#4238,1.2);
#848=CYLINDRICAL_SURFACE('',#4240,3.25);
#849=CYLINDRICAL_SURFACE('',#4242,0.9);
#850=CYLINDRICAL_SURFACE('',#4246,0.9);
#851=CYLINDRICAL_SURFACE('',#4250,0.9);
#852=CYLINDRICAL_SURFACE('',#4256,0.9);
#853=CYLINDRICAL_SURFACE('',#4260,0.425);
#854=CYLINDRICAL_SURFACE('',#4263,0.425);
#855=CYLINDRICAL_SURFACE('',#4266,0.425);
#856=CYLINDRICAL_SURFACE('',#4269,1.);
#857=CYLINDRICAL_SURFACE('',#4282,1.1);
#858=CYLINDRICAL_SURFACE('',#4285,0.425);
#859=CYLINDRICAL_SURFACE('',#4288,0.425);
#860=CYLINDRICAL_SURFACE('',#4298,0.425);
#861=CYLINDRICAL_SURFACE('',#4301,1.);
#862=CYLINDRICAL_SURFACE('',#4307,0.34);
#863=CYLINDRICAL_SURFACE('',#4314,1.5);
#864=CYLINDRICAL_SURFACE('',#4317,1.);
#865=CYLINDRICAL_SURFACE('',#4321,0.425);
#866=CYLINDRICAL_SURFACE('',#4324,1.5);
#867=CYLINDRICAL_SURFACE('',#4330,1.005);
#868=CYLINDRICAL_SURFACE('',#4333,1.4);
#869=CYLINDRICAL_SURFACE('',#4339,0.81);
#870=CYLINDRICAL_SURFACE('',#4342,1.1);
#871=CYLINDRICAL_SURFACE('',#4348,1.005);
#872=CYLINDRICAL_SURFACE('',#4351,1.4);
#873=CYLINDRICAL_SURFACE('',#4368,0.4);
#874=CYLINDRICAL_SURFACE('',#4375,0.65);
#875=CYLINDRICAL_SURFACE('',#4383,0.3933);
#876=CYLINDRICAL_SURFACE('',#4385,0.42);
#877=CYLINDRICAL_SURFACE('',#4388,0.8);
#878=CYLINDRICAL_SURFACE('',#4401,0.338975);
#879=CYLINDRICAL_SURFACE('',#4414,0.65);
#880=CYLINDRICAL_SURFACE('',#4422,0.3933);
#881=CYLINDRICAL_SURFACE('',#4460,0.165);
#882=CYLINDRICAL_SURFACE('',#4463,0.165);
#883=CYLINDRICAL_SURFACE('',#4466,0.165);
#884=CYLINDRICAL_SURFACE('',#4469,0.165);
#885=CYLINDRICAL_SURFACE('',#4477,5.);
#886=CYLINDRICAL_SURFACE('',#4484,5.);
#887=CYLINDRICAL_SURFACE('',#4485,3.);
#888=CYLINDRICAL_SURFACE('',#4487,2.35);
#889=CYLINDRICAL_SURFACE('',#4490,3.);
#890=CYLINDRICAL_SURFACE('',#4495,1.9);
#891=CYLINDRICAL_SURFACE('',#4498,2.34);
#892=CYLINDRICAL_SURFACE('',#4511,1.63531);
#893=CYLINDRICAL_SURFACE('',#4513,1.);
#894=CYLINDRICAL_SURFACE('',#4519,1.63531);
#895=CYLINDRICAL_SURFACE('',#4531,1.71469);
#896=CYLINDRICAL_SURFACE('',#4538,2.35);
#897=CYLINDRICAL_SURFACE('',#4543,1.71469);
#898=CYLINDRICAL_SURFACE('',#4565,1.706752);
#899=CYLINDRICAL_SURFACE('',#4605,1.643248);
#900=CYLINDRICAL_SURFACE('',#4619,1.70469);
#901=CYLINDRICAL_SURFACE('',#4623,1.65031);
#902=CYLINDRICAL_SURFACE('',#4627,1.70469);
#903=CYLINDRICAL_SURFACE('',#4631,1.65031);
#904=CYLINDRICAL_SURFACE('',#4638,0.225);
#905=CYLINDRICAL_SURFACE('',#4641,0.225);
#906=CYLINDRICAL_SURFACE('',#4644,0.225);
#907=CYLINDRICAL_SURFACE('',#4647,0.225);
#908=CYLINDRICAL_SURFACE('',#4650,2.34);
#909=CYLINDRICAL_SURFACE('',#4655,1.9);
#910=CYLINDRICAL_SURFACE('',#4657,3.);
#911=CYLINDRICAL_SURFACE('',#4677,0.35);
#912=CYLINDRICAL_SURFACE('',#4685,0.1954);
#913=CYLINDRICAL_SURFACE('',#4708,1.3);
#914=CYLINDRICAL_SURFACE('',#4709,0.8);
#915=CYLINDRICAL_SURFACE('',#4713,0.8);
#916=CYLINDRICAL_SURFACE('',#4723,2.);
#917=CYLINDRICAL_SURFACE('',#4729,3.5);
#918=CYLINDRICAL_SURFACE('',#4731,0.81);
#919=CYLINDRICAL_SURFACE('',#4734,1.5);
#920=CYLINDRICAL_SURFACE('',#4740,0.7);
#921=FACE_BOUND('',#1238,.T.);
#922=FACE_BOUND('',#1248,.T.);
#923=FACE_BOUND('',#1263,.T.);
#924=FACE_BOUND('',#1264,.T.);
#925=FACE_BOUND('',#1265,.T.);
#926=FACE_BOUND('',#1266,.T.);
#927=FACE_BOUND('',#1268,.T.);
#928=FACE_BOUND('',#1269,.T.);
#929=FACE_BOUND('',#1270,.T.);
#930=FACE_BOUND('',#1271,.T.);
#931=FACE_BOUND('',#1272,.T.);
#932=FACE_BOUND('',#1273,.T.);
#933=FACE_BOUND('',#1274,.T.);
#934=FACE_BOUND('',#1275,.T.);
#935=FACE_BOUND('',#1280,.T.);
#936=FACE_BOUND('',#1281,.T.);
#937=FACE_BOUND('',#1284,.T.);
#938=FACE_BOUND('',#1285,.T.);
#939=FACE_BOUND('',#1288,.T.);
#940=FACE_BOUND('',#1290,.T.);
#941=FACE_BOUND('',#1294,.T.);
#942=FACE_BOUND('',#1296,.T.);
#943=FACE_BOUND('',#1300,.T.);
#944=FACE_BOUND('',#1305,.T.);
#945=FACE_BOUND('',#1309,.T.);
#946=FACE_BOUND('',#1311,.T.);
#947=FACE_BOUND('',#1315,.T.);
#948=FACE_BOUND('',#1317,.T.);
#949=FACE_BOUND('',#1321,.T.);
#950=FACE_BOUND('',#1323,.T.);
#951=FACE_BOUND('',#1327,.T.);
#952=FACE_BOUND('',#1329,.T.);
#953=FACE_BOUND('',#1339,.T.);
#954=FACE_BOUND('',#1347,.T.);
#955=FACE_BOUND('',#1353,.T.);
#956=FACE_BOUND('',#1355,.T.);
#957=FACE_BOUND('',#1366,.T.);
#958=FACE_BOUND('',#1368,.T.);
#959=FACE_BOUND('',#1374,.T.);
#960=FACE_BOUND('',#1395,.T.);
#961=FACE_BOUND('',#1397,.T.);
#962=FACE_BOUND('',#1403,.T.);
#963=FACE_BOUND('',#1404,.T.);
#964=FACE_BOUND('',#1405,.T.);
#965=FACE_BOUND('',#1406,.T.);
#966=FACE_BOUND('',#1407,.T.);
#967=FACE_BOUND('',#1409,.T.);
#968=FACE_BOUND('',#1410,.T.);
#969=FACE_BOUND('',#1411,.T.);
#970=FACE_BOUND('',#1412,.T.);
#971=FACE_BOUND('',#1413,.T.);
#972=FACE_BOUND('',#1417,.T.);
#973=FACE_BOUND('',#1419,.T.);
#974=FACE_BOUND('',#1425,.T.);
#975=FACE_BOUND('',#1428,.T.);
#976=FACE_BOUND('',#1433,.T.);
#977=FACE_BOUND('',#1438,.T.);
#978=FACE_BOUND('',#1466,.T.);
#979=FACE_BOUND('',#1469,.T.);
#980=FACE_BOUND('',#1472,.T.);
#981=FACE_BOUND('',#1475,.T.);
#982=FACE_BOUND('',#1478,.T.);
#983=FACE_BOUND('',#1486,.T.);
#984=FACE_BOUND('',#1490,.T.);
#985=FACE_BOUND('',#1491,.T.);
#986=FACE_BOUND('',#1492,.T.);
#987=FACE_BOUND('',#1493,.T.);
#988=FACE_BOUND('',#1494,.T.);
#989=FACE_BOUND('',#1496,.T.);
#990=FACE_BOUND('',#1497,.T.);
#991=FACE_BOUND('',#1498,.T.);
#992=FACE_BOUND('',#1499,.T.);
#993=FACE_BOUND('',#1500,.T.);
#994=FACE_BOUND('',#1515,.T.);
#995=FACE_BOUND('',#1519,.T.);
#996=FACE_BOUND('',#1521,.T.);
#997=FACE_BOUND('',#1539,.T.);
#998=FACE_BOUND('',#1541,.T.);
#999=FACE_BOUND('',#1550,.T.);
#1000=FACE_BOUND('',#1552,.T.);
#1001=FACE_OUTER_BOUND('',#1237,.T.);
#1002=FACE_OUTER_BOUND('',#1239,.T.);
#1003=FACE_OUTER_BOUND('',#1240,.T.);
#1004=FACE_OUTER_BOUND('',#1241,.T.);
#1005=FACE_OUTER_BOUND('',#1242,.T.);
#1006=FACE_OUTER_BOUND('',#1243,.T.);
#1007=FACE_OUTER_BOUND('',#1244,.T.);
#1008=FACE_OUTER_BOUND('',#1245,.T.);
#1009=FACE_OUTER_BOUND('',#1246,.T.);
#1010=FACE_OUTER_BOUND('',#1247,.T.);
#1011=FACE_OUTER_BOUND('',#1249,.T.);
#1012=FACE_OUTER_BOUND('',#1250,.T.);
#1013=FACE_OUTER_BOUND('',#1251,.T.);
#1014=FACE_OUTER_BOUND('',#1252,.T.);
#1015=FACE_OUTER_BOUND('',#1253,.T.);
#1016=FACE_OUTER_BOUND('',#1254,.T.);
#1017=FACE_OUTER_BOUND('',#1255,.T.);
#1018=FACE_OUTER_BOUND('',#1256,.T.);
#1019=FACE_OUTER_BOUND('',#1257,.T.);
#1020=FACE_OUTER_BOUND('',#1258,.T.);
#1021=FACE_OUTER_BOUND('',#1259,.T.);
#1022=FACE_OUTER_BOUND('',#1260,.T.);
#1023=FACE_OUTER_BOUND('',#1261,.T.);
#1024=FACE_OUTER_BOUND('',#1262,.T.);
#1025=FACE_OUTER_BOUND('',#1267,.T.);
#1026=FACE_OUTER_BOUND('',#1276,.T.);
#1027=FACE_OUTER_BOUND('',#1277,.T.);
#1028=FACE_OUTER_BOUND('',#1278,.T.);
#1029=FACE_OUTER_BOUND('',#1279,.T.);
#1030=FACE_OUTER_BOUND('',#1282,.T.);
#1031=FACE_OUTER_BOUND('',#1283,.T.);
#1032=FACE_OUTER_BOUND('',#1286,.T.);
#1033=FACE_OUTER_BOUND('',#1287,.T.);
#1034=FACE_OUTER_BOUND('',#1289,.T.);
#1035=FACE_OUTER_BOUND('',#1291,.T.);
#1036=FACE_OUTER_BOUND('',#1292,.T.);
#1037=FACE_OUTER_BOUND('',#1293,.T.);
#1038=FACE_OUTER_BOUND('',#1295,.T.);
#1039=FACE_OUTER_BOUND('',#1297,.T.);
#1040=FACE_OUTER_BOUND('',#1298,.T.);
#1041=FACE_OUTER_BOUND('',#1299,.T.);
#1042=FACE_OUTER_BOUND('',#1301,.T.);
#1043=FACE_OUTER_BOUND('',#1302,.T.);
#1044=FACE_OUTER_BOUND('',#1303,.T.);
#1045=FACE_OUTER_BOUND('',#1304,.T.);
#1046=FACE_OUTER_BOUND('',#1306,.T.);
#1047=FACE_OUTER_BOUND('',#1307,.T.);
#1048=FACE_OUTER_BOUND('',#1308,.T.);
#1049=FACE_OUTER_BOUND('',#1310,.T.);
#1050=FACE_OUTER_BOUND('',#1312,.T.);
#1051=FACE_OUTER_BOUND('',#1313,.T.);
#1052=FACE_OUTER_BOUND('',#1314,.T.);
#1053=FACE_OUTER_BOUND('',#1316,.T.);
#1054=FACE_OUTER_BOUND('',#1318,.T.);
#1055=FACE_OUTER_BOUND('',#1319,.T.);
#1056=FACE_OUTER_BOUND('',#1320,.T.);
#1057=FACE_OUTER_BOUND('',#1322,.T.);
#1058=FACE_OUTER_BOUND('',#1324,.T.);
#1059=FACE_OUTER_BOUND('',#1325,.T.);
#1060=FACE_OUTER_BOUND('',#1326,.T.);
#1061=FACE_OUTER_BOUND('',#1328,.T.);
#1062=FACE_OUTER_BOUND('',#1330,.T.);
#1063=FACE_OUTER_BOUND('',#1331,.T.);
#1064=FACE_OUTER_BOUND('',#1332,.T.);
#1065=FACE_OUTER_BOUND('',#1333,.T.);
#1066=FACE_OUTER_BOUND('',#1334,.T.);
#1067=FACE_OUTER_BOUND('',#1335,.T.);
#1068=FACE_OUTER_BOUND('',#1336,.T.);
#1069=FACE_OUTER_BOUND('',#1337,.T.);
#1070=FACE_OUTER_BOUND('',#1338,.T.);
#1071=FACE_OUTER_BOUND('',#1340,.T.);
#1072=FACE_OUTER_BOUND('',#1341,.T.);
#1073=FACE_OUTER_BOUND('',#1342,.T.);
#1074=FACE_OUTER_BOUND('',#1343,.T.);
#1075=FACE_OUTER_BOUND('',#1344,.T.);
#1076=FACE_OUTER_BOUND('',#1345,.T.);
#1077=FACE_OUTER_BOUND('',#1346,.T.);
#1078=FACE_OUTER_BOUND('',#1348,.T.);
#1079=FACE_OUTER_BOUND('',#1349,.T.);
#1080=FACE_OUTER_BOUND('',#1350,.T.);
#1081=FACE_OUTER_BOUND('',#1351,.T.);
#1082=FACE_OUTER_BOUND('',#1352,.T.);
#1083=FACE_OUTER_BOUND('',#1354,.T.);
#1084=FACE_OUTER_BOUND('',#1356,.T.);
#1085=FACE_OUTER_BOUND('',#1357,.T.);
#1086=FACE_OUTER_BOUND('',#1358,.T.);
#1087=FACE_OUTER_BOUND('',#1359,.T.);
#1088=FACE_OUTER_BOUND('',#1360,.T.);
#1089=FACE_OUTER_BOUND('',#1361,.T.);
#1090=FACE_OUTER_BOUND('',#1362,.T.);
#1091=FACE_OUTER_BOUND('',#1363,.T.);
#1092=FACE_OUTER_BOUND('',#1364,.T.);
#1093=FACE_OUTER_BOUND('',#1365,.T.);
#1094=FACE_OUTER_BOUND('',#1367,.T.);
#1095=FACE_OUTER_BOUND('',#1369,.T.);
#1096=FACE_OUTER_BOUND('',#1370,.T.);
#1097=FACE_OUTER_BOUND('',#1371,.T.);
#1098=FACE_OUTER_BOUND('',#1372,.T.);
#1099=FACE_OUTER_BOUND('',#1373,.T.);
#1100=FACE_OUTER_BOUND('',#1375,.T.);
#1101=FACE_OUTER_BOUND('',#1376,.T.);
#1102=FACE_OUTER_BOUND('',#1377,.T.);
#1103=FACE_OUTER_BOUND('',#1378,.T.);
#1104=FACE_OUTER_BOUND('',#1379,.T.);
#1105=FACE_OUTER_BOUND('',#1380,.T.);
#1106=FACE_OUTER_BOUND('',#1381,.T.);
#1107=FACE_OUTER_BOUND('',#1382,.T.);
#1108=FACE_OUTER_BOUND('',#1383,.T.);
#1109=FACE_OUTER_BOUND('',#1384,.T.);
#1110=FACE_OUTER_BOUND('',#1385,.T.);
#1111=FACE_OUTER_BOUND('',#1386,.T.);
#1112=FACE_OUTER_BOUND('',#1387,.T.);
#1113=FACE_OUTER_BOUND('',#1388,.T.);
#1114=FACE_OUTER_BOUND('',#1389,.T.);
#1115=FACE_OUTER_BOUND('',#1390,.T.);
#1116=FACE_OUTER_BOUND('',#1391,.T.);
#1117=FACE_OUTER_BOUND('',#1392,.T.);
#1118=FACE_OUTER_BOUND('',#1393,.T.);
#1119=FACE_OUTER_BOUND('',#1394,.T.);
#1120=FACE_OUTER_BOUND('',#1396,.T.);
#1121=FACE_OUTER_BOUND('',#1398,.T.);
#1122=FACE_OUTER_BOUND('',#1399,.T.);
#1123=FACE_OUTER_BOUND('',#1400,.T.);
#1124=FACE_OUTER_BOUND('',#1401,.T.);
#1125=FACE_OUTER_BOUND('',#1402,.T.);
#1126=FACE_OUTER_BOUND('',#1408,.T.);
#1127=FACE_OUTER_BOUND('',#1414,.T.);
#1128=FACE_OUTER_BOUND('',#1415,.T.);
#1129=FACE_OUTER_BOUND('',#1416,.T.);
#1130=FACE_OUTER_BOUND('',#1418,.T.);
#1131=FACE_OUTER_BOUND('',#1420,.T.);
#1132=FACE_OUTER_BOUND('',#1421,.T.);
#1133=FACE_OUTER_BOUND('',#1422,.T.);
#1134=FACE_OUTER_BOUND('',#1423,.T.);
#1135=FACE_OUTER_BOUND('',#1424,.T.);
#1136=FACE_OUTER_BOUND('',#1426,.T.);
#1137=FACE_OUTER_BOUND('',#1427,.T.);
#1138=FACE_OUTER_BOUND('',#1429,.T.);
#1139=FACE_OUTER_BOUND('',#1430,.T.);
#1140=FACE_OUTER_BOUND('',#1431,.T.);
#1141=FACE_OUTER_BOUND('',#1432,.T.);
#1142=FACE_OUTER_BOUND('',#1434,.T.);
#1143=FACE_OUTER_BOUND('',#1435,.T.);
#1144=FACE_OUTER_BOUND('',#1436,.T.);
#1145=FACE_OUTER_BOUND('',#1437,.T.);
#1146=FACE_OUTER_BOUND('',#1439,.T.);
#1147=FACE_OUTER_BOUND('',#1440,.T.);
#1148=FACE_OUTER_BOUND('',#1441,.T.);
#1149=FACE_OUTER_BOUND('',#1442,.T.);
#1150=FACE_OUTER_BOUND('',#1443,.T.);
#1151=FACE_OUTER_BOUND('',#1444,.T.);
#1152=FACE_OUTER_BOUND('',#1445,.T.);
#1153=FACE_OUTER_BOUND('',#1446,.T.);
#1154=FACE_OUTER_BOUND('',#1447,.T.);
#1155=FACE_OUTER_BOUND('',#1448,.T.);
#1156=FACE_OUTER_BOUND('',#1449,.T.);
#1157=FACE_OUTER_BOUND('',#1450,.T.);
#1158=FACE_OUTER_BOUND('',#1451,.T.);
#1159=FACE_OUTER_BOUND('',#1452,.T.);
#1160=FACE_OUTER_BOUND('',#1453,.T.);
#1161=FACE_OUTER_BOUND('',#1454,.T.);
#1162=FACE_OUTER_BOUND('',#1455,.T.);
#1163=FACE_OUTER_BOUND('',#1456,.T.);
#1164=FACE_OUTER_BOUND('',#1457,.T.);
#1165=FACE_OUTER_BOUND('',#1458,.T.);
#1166=FACE_OUTER_BOUND('',#1459,.T.);
#1167=FACE_OUTER_BOUND('',#1460,.T.);
#1168=FACE_OUTER_BOUND('',#1461,.T.);
#1169=FACE_OUTER_BOUND('',#1462,.T.);
#1170=FACE_OUTER_BOUND('',#1463,.T.);
#1171=FACE_OUTER_BOUND('',#1464,.T.);
#1172=FACE_OUTER_BOUND('',#1465,.T.);
#1173=FACE_OUTER_BOUND('',#1467,.T.);
#1174=FACE_OUTER_BOUND('',#1468,.T.);
#1175=FACE_OUTER_BOUND('',#1470,.T.);
#1176=FACE_OUTER_BOUND('',#1471,.T.);
#1177=FACE_OUTER_BOUND('',#1473,.T.);
#1178=FACE_OUTER_BOUND('',#1474,.T.);
#1179=FACE_OUTER_BOUND('',#1476,.T.);
#1180=FACE_OUTER_BOUND('',#1477,.T.);
#1181=FACE_OUTER_BOUND('',#1479,.T.);
#1182=FACE_OUTER_BOUND('',#1480,.T.);
#1183=FACE_OUTER_BOUND('',#1481,.T.);
#1184=FACE_OUTER_BOUND('',#1482,.T.);
#1185=FACE_OUTER_BOUND('',#1483,.T.);
#1186=FACE_OUTER_BOUND('',#1484,.T.);
#1187=FACE_OUTER_BOUND('',#1485,.T.);
#1188=FACE_OUTER_BOUND('',#1487,.T.);
#1189=FACE_OUTER_BOUND('',#1488,.T.);
#1190=FACE_OUTER_BOUND('',#1489,.T.);
#1191=FACE_OUTER_BOUND('',#1495,.T.);
#1192=FACE_OUTER_BOUND('',#1501,.T.);
#1193=FACE_OUTER_BOUND('',#1502,.T.);
#1194=FACE_OUTER_BOUND('',#1503,.T.);
#1195=FACE_OUTER_BOUND('',#1504,.T.);
#1196=FACE_OUTER_BOUND('',#1505,.T.);
#1197=FACE_OUTER_BOUND('',#1506,.T.);
#1198=FACE_OUTER_BOUND('',#1507,.T.);
#1199=FACE_OUTER_BOUND('',#1508,.T.);
#1200=FACE_OUTER_BOUND('',#1509,.T.);
#1201=FACE_OUTER_BOUND('',#1510,.T.);
#1202=FACE_OUTER_BOUND('',#1511,.T.);
#1203=FACE_OUTER_BOUND('',#1512,.T.);
#1204=FACE_OUTER_BOUND('',#1513,.T.);
#1205=FACE_OUTER_BOUND('',#1514,.T.);
#1206=FACE_OUTER_BOUND('',#1516,.T.);
#1207=FACE_OUTER_BOUND('',#1517,.T.);
#1208=FACE_OUTER_BOUND('',#1518,.T.);
#1209=FACE_OUTER_BOUND('',#1520,.T.);
#1210=FACE_OUTER_BOUND('',#1522,.T.);
#1211=FACE_OUTER_BOUND('',#1523,.T.);
#1212=FACE_OUTER_BOUND('',#1524,.T.);
#1213=FACE_OUTER_BOUND('',#1525,.T.);
#1214=FACE_OUTER_BOUND('',#1526,.T.);
#1215=FACE_OUTER_BOUND('',#1527,.T.);
#1216=FACE_OUTER_BOUND('',#1528,.T.);
#1217=FACE_OUTER_BOUND('',#1529,.T.);
#1218=FACE_OUTER_BOUND('',#1530,.T.);
#1219=FACE_OUTER_BOUND('',#1531,.T.);
#1220=FACE_OUTER_BOUND('',#1532,.T.);
#1221=FACE_OUTER_BOUND('',#1533,.T.);
#1222=FACE_OUTER_BOUND('',#1534,.T.);
#1223=FACE_OUTER_BOUND('',#1535,.T.);
#1224=FACE_OUTER_BOUND('',#1536,.T.);
#1225=FACE_OUTER_BOUND('',#1537,.T.);
#1226=FACE_OUTER_BOUND('',#1538,.T.);
#1227=FACE_OUTER_BOUND('',#1540,.T.);
#1228=FACE_OUTER_BOUND('',#1542,.T.);
#1229=FACE_OUTER_BOUND('',#1543,.T.);
#1230=FACE_OUTER_BOUND('',#1544,.T.);
#1231=FACE_OUTER_BOUND('',#1545,.T.);
#1232=FACE_OUTER_BOUND('',#1546,.T.);
#1233=FACE_OUTER_BOUND('',#1547,.T.);
#1234=FACE_OUTER_BOUND('',#1548,.T.);
#1235=FACE_OUTER_BOUND('',#1549,.T.);
#1236=FACE_OUTER_BOUND('',#1551,.T.);
#1237=EDGE_LOOP('',(#2590,#2591,#2592,#2593,#2594,#2595,#2596,#2597));
#1238=EDGE_LOOP('',(#2598));
#1239=EDGE_LOOP('',(#2599,#2600,#2601,#2602));
#1240=EDGE_LOOP('',(#2603,#2604,#2605,#2606));
#1241=EDGE_LOOP('',(#2607,#2608,#2609,#2610));
#1242=EDGE_LOOP('',(#2611,#2612,#2613,#2614));
#1243=EDGE_LOOP('',(#2615,#2616,#2617,#2618));
#1244=EDGE_LOOP('',(#2619,#2620,#2621,#2622,#2623,#2624,#2625,#2626));
#1245=EDGE_LOOP('',(#2627,#2628,#2629,#2630,#2631,#2632,#2633,#2634));
#1246=EDGE_LOOP('',(#2635,#2636,#2637,#2638,#2639,#2640,#2641,#2642));
#1247=EDGE_LOOP('',(#2643));
#1248=EDGE_LOOP('',(#2644));
#1249=EDGE_LOOP('',(#2645,#2646,#2647,#2648,#2649,#2650,#2651,#2652));
#1250=EDGE_LOOP('',(#2653,#2654,#2655,#2656));
#1251=EDGE_LOOP('',(#2657,#2658,#2659,#2660));
#1252=EDGE_LOOP('',(#2661,#2662,#2663,#2664));
#1253=EDGE_LOOP('',(#2665,#2666,#2667,#2668));
#1254=EDGE_LOOP('',(#2669,#2670,#2671,#2672));
#1255=EDGE_LOOP('',(#2673,#2674,#2675,#2676));
#1256=EDGE_LOOP('',(#2677,#2678,#2679,#2680));
#1257=EDGE_LOOP('',(#2681,#2682,#2683,#2684));
#1258=EDGE_LOOP('',(#2685,#2686,#2687,#2688));
#1259=EDGE_LOOP('',(#2689,#2690,#2691,#2692));
#1260=EDGE_LOOP('',(#2693,#2694,#2695,#2696));
#1261=EDGE_LOOP('',(#2697,#2698,#2699,#2700));
#1262=EDGE_LOOP('',(#2701,#2702,#2703,#2704,#2705,#2706,#2707,#2708));
#1263=EDGE_LOOP('',(#2709,#2710,#2711,#2712,#2713,#2714,#2715,#2716,#2717,
#2718,#2719,#2720));
#1264=EDGE_LOOP('',(#2721));
#1265=EDGE_LOOP('',(#2722));
#1266=EDGE_LOOP('',(#2723));
#1267=EDGE_LOOP('',(#2724,#2725,#2726,#2727,#2728,#2729,#2730,#2731));
#1268=EDGE_LOOP('',(#2732));
#1269=EDGE_LOOP('',(#2733));
#1270=EDGE_LOOP('',(#2734));
#1271=EDGE_LOOP('',(#2735));
#1272=EDGE_LOOP('',(#2736));
#1273=EDGE_LOOP('',(#2737));
#1274=EDGE_LOOP('',(#2738));
#1275=EDGE_LOOP('',(#2739));
#1276=EDGE_LOOP('',(#2740,#2741,#2742,#2743));
#1277=EDGE_LOOP('',(#2744,#2745,#2746,#2747));
#1278=EDGE_LOOP('',(#2748,#2749,#2750,#2751));
#1279=EDGE_LOOP('',(#2752,#2753,#2754,#2755));
#1280=EDGE_LOOP('',(#2756));
#1281=EDGE_LOOP('',(#2757));
#1282=EDGE_LOOP('',(#2758,#2759,#2760,#2761));
#1283=EDGE_LOOP('',(#2762,#2763,#2764,#2765));
#1284=EDGE_LOOP('',(#2766));
#1285=EDGE_LOOP('',(#2767));
#1286=EDGE_LOOP('',(#2768,#2769,#2770,#2771));
#1287=EDGE_LOOP('',(#2772,#2773,#2774,#2775));
#1288=EDGE_LOOP('',(#2776));
#1289=EDGE_LOOP('',(#2777,#2778,#2779,#2780));
#1290=EDGE_LOOP('',(#2781));
#1291=EDGE_LOOP('',(#2782,#2783,#2784,#2785));
#1292=EDGE_LOOP('',(#2786,#2787,#2788,#2789));
#1293=EDGE_LOOP('',(#2790));
#1294=EDGE_LOOP('',(#2791));
#1295=EDGE_LOOP('',(#2792));
#1296=EDGE_LOOP('',(#2793));
#1297=EDGE_LOOP('',(#2794,#2795,#2796,#2797));
#1298=EDGE_LOOP('',(#2798));
#1299=EDGE_LOOP('',(#2799));
#1300=EDGE_LOOP('',(#2800));
#1301=EDGE_LOOP('',(#2801,#2802,#2803,#2804));
#1302=EDGE_LOOP('',(#2805));
#1303=EDGE_LOOP('',(#2806,#2807,#2808,#2809));
#1304=EDGE_LOOP('',(#2810));
#1305=EDGE_LOOP('',(#2811));
#1306=EDGE_LOOP('',(#2812,#2813,#2814,#2815));
#1307=EDGE_LOOP('',(#2816,#2817,#2818,#2819));
#1308=EDGE_LOOP('',(#2820));
#1309=EDGE_LOOP('',(#2821));
#1310=EDGE_LOOP('',(#2822));
#1311=EDGE_LOOP('',(#2823));
#1312=EDGE_LOOP('',(#2824,#2825,#2826,#2827));
#1313=EDGE_LOOP('',(#2828,#2829,#2830,#2831));
#1314=EDGE_LOOP('',(#2832));
#1315=EDGE_LOOP('',(#2833));
#1316=EDGE_LOOP('',(#2834));
#1317=EDGE_LOOP('',(#2835));
#1318=EDGE_LOOP('',(#2836,#2837,#2838,#2839));
#1319=EDGE_LOOP('',(#2840,#2841,#2842,#2843));
#1320=EDGE_LOOP('',(#2844));
#1321=EDGE_LOOP('',(#2845));
#1322=EDGE_LOOP('',(#2846));
#1323=EDGE_LOOP('',(#2847));
#1324=EDGE_LOOP('',(#2848,#2849,#2850,#2851));
#1325=EDGE_LOOP('',(#2852,#2853,#2854,#2855));
#1326=EDGE_LOOP('',(#2856));
#1327=EDGE_LOOP('',(#2857));
#1328=EDGE_LOOP('',(#2858));
#1329=EDGE_LOOP('',(#2859));
#1330=EDGE_LOOP('',(#2860,#2861,#2862,#2863));
#1331=EDGE_LOOP('',(#2864,#2865,#2866,#2867));
#1332=EDGE_LOOP('',(#2868,#2869,#2870,#2871));
#1333=EDGE_LOOP('',(#2872,#2873,#2874,#2875));
#1334=EDGE_LOOP('',(#2876,#2877,#2878,#2879));
#1335=EDGE_LOOP('',(#2880,#2881,#2882,#2883));
#1336=EDGE_LOOP('',(#2884,#2885,#2886,#2887,#2888,#2889));
#1337=EDGE_LOOP('',(#2890,#2891,#2892,#2893,#2894,#2895));
#1338=EDGE_LOOP('',(#2896));
#1339=EDGE_LOOP('',(#2897));
#1340=EDGE_LOOP('',(#2898,#2899,#2900,#2901));
#1341=EDGE_LOOP('',(#2902));
#1342=EDGE_LOOP('',(#2903));
#1343=EDGE_LOOP('',(#2904,#2905,#2906,#2907));
#1344=EDGE_LOOP('',(#2908,#2909,#2910,#2911));
#1345=EDGE_LOOP('',(#2912,#2913,#2914,#2915));
#1346=EDGE_LOOP('',(#2916));
#1347=EDGE_LOOP('',(#2917));
#1348=EDGE_LOOP('',(#2918,#2919,#2920,#2921));
#1349=EDGE_LOOP('',(#2922,#2923,#2924,#2925));
#1350=EDGE_LOOP('',(#2926,#2927,#2928,#2929));
#1351=EDGE_LOOP('',(#2930,#2931,#2932,#2933));
#1352=EDGE_LOOP('',(#2934));
#1353=EDGE_LOOP('',(#2935));
#1354=EDGE_LOOP('',(#2936));
#1355=EDGE_LOOP('',(#2937));
#1356=EDGE_LOOP('',(#2938,#2939,#2940,#2941,#2942,#2943,#2944,#2945,#2946));
#1357=EDGE_LOOP('',(#2947,#2948,#2949,#2950,#2951,#2952,#2953,#2954,#2955));
#1358=EDGE_LOOP('',(#2956,#2957,#2958,#2959));
#1359=EDGE_LOOP('',(#2960,#2961,#2962,#2963));
#1360=EDGE_LOOP('',(#2964,#2965,#2966,#2967));
#1361=EDGE_LOOP('',(#2968,#2969,#2970,#2971));
#1362=EDGE_LOOP('',(#2972,#2973,#2974,#2975));
#1363=EDGE_LOOP('',(#2976,#2977,#2978,#2979));
#1364=EDGE_LOOP('',(#2980,#2981,#2982,#2983));
#1365=EDGE_LOOP('',(#2984));
#1366=EDGE_LOOP('',(#2985));
#1367=EDGE_LOOP('',(#2986));
#1368=EDGE_LOOP('',(#2987));
#1369=EDGE_LOOP('',(#2988));
#1370=EDGE_LOOP('',(#2989,#2990,#2991,#2992));
#1371=EDGE_LOOP('',(#2993,#2994,#2995,#2996));
#1372=EDGE_LOOP('',(#2997,#2998,#2999,#3000));
#1373=EDGE_LOOP('',(#3001));
#1374=EDGE_LOOP('',(#3002));
#1375=EDGE_LOOP('',(#3003,#3004,#3005,#3006));
#1376=EDGE_LOOP('',(#3007,#3008,#3009,#3010));
#1377=EDGE_LOOP('',(#3011,#3012,#3013,#3014));
#1378=EDGE_LOOP('',(#3015));
#1379=EDGE_LOOP('',(#3016,#3017,#3018,#3019));
#1380=EDGE_LOOP('',(#3020,#3021,#3022,#3023));
#1381=EDGE_LOOP('',(#3024,#3025,#3026,#3027));
#1382=EDGE_LOOP('',(#3028,#3029,#3030,#3031));
#1383=EDGE_LOOP('',(#3032,#3033,#3034,#3035));
#1384=EDGE_LOOP('',(#3036,#3037,#3038,#3039));
#1385=EDGE_LOOP('',(#3040,#3041,#3042,#3043,#3044,#3045));
#1386=EDGE_LOOP('',(#3046,#3047,#3048,#3049,#3050,#3051));
#1387=EDGE_LOOP('',(#3052,#3053,#3054,#3055));
#1388=EDGE_LOOP('',(#3056,#3057,#3058,#3059));
#1389=EDGE_LOOP('',(#3060,#3061,#3062,#3063));
#1390=EDGE_LOOP('',(#3064,#3065,#3066,#3067));
#1391=EDGE_LOOP('',(#3068,#3069,#3070,#3071));
#1392=EDGE_LOOP('',(#3072,#3073,#3074,#3075));
#1393=EDGE_LOOP('',(#3076,#3077,#3078,#3079));
#1394=EDGE_LOOP('',(#3080));
#1395=EDGE_LOOP('',(#3081));
#1396=EDGE_LOOP('',(#3082));
#1397=EDGE_LOOP('',(#3083));
#1398=EDGE_LOOP('',(#3084,#3085,#3086,#3087));
#1399=EDGE_LOOP('',(#3088,#3089,#3090,#3091));
#1400=EDGE_LOOP('',(#3092,#3093,#3094,#3095));
#1401=EDGE_LOOP('',(#3096,#3097,#3098,#3099));
#1402=EDGE_LOOP('',(#3100));
#1403=EDGE_LOOP('',(#3101));
#1404=EDGE_LOOP('',(#3102));
#1405=EDGE_LOOP('',(#3103));
#1406=EDGE_LOOP('',(#3104));
#1407=EDGE_LOOP('',(#3105));
#1408=EDGE_LOOP('',(#3106));
#1409=EDGE_LOOP('',(#3107));
#1410=EDGE_LOOP('',(#3108));
#1411=EDGE_LOOP('',(#3109));
#1412=EDGE_LOOP('',(#3110));
#1413=EDGE_LOOP('',(#3111));
#1414=EDGE_LOOP('',(#3112,#3113,#3114,#3115));
#1415=EDGE_LOOP('',(#3116,#3117,#3118,#3119));
#1416=EDGE_LOOP('',(#3120));
#1417=EDGE_LOOP('',(#3121));
#1418=EDGE_LOOP('',(#3122));
#1419=EDGE_LOOP('',(#3123));
#1420=EDGE_LOOP('',(#3124,#3125,#3126,#3127,#3128,#3129));
#1421=EDGE_LOOP('',(#3130,#3131,#3132,#3133,#3134));
#1422=EDGE_LOOP('',(#3135,#3136,#3137,#3138));
#1423=EDGE_LOOP('',(#3139,#3140,#3141,#3142));
#1424=EDGE_LOOP('',(#3143));
#1425=EDGE_LOOP('',(#3144));
#1426=EDGE_LOOP('',(#3145,#3146,#3147,#3148,#3149));
#1427=EDGE_LOOP('',(#3150));
#1428=EDGE_LOOP('',(#3151));
#1429=EDGE_LOOP('',(#3152,#3153,#3154,#3155));
#1430=EDGE_LOOP('',(#3156,#3157,#3158,#3159,#3160,#3161));
#1431=EDGE_LOOP('',(#3162,#3163,#3164,#3165,#3166));
#1432=EDGE_LOOP('',(#3167));
#1433=EDGE_LOOP('',(#3168));
#1434=EDGE_LOOP('',(#3169,#3170,#3171,#3172));
#1435=EDGE_LOOP('',(#3173,#3174,#3175,#3176));
#1436=EDGE_LOOP('',(#3177,#3178,#3179,#3180));
#1437=EDGE_LOOP('',(#3181));
#1438=EDGE_LOOP('',(#3182));
#1439=EDGE_LOOP('',(#3183,#3184,#3185,#3186,#3187));
#1440=EDGE_LOOP('',(#3188,#3189));
#1441=EDGE_LOOP('',(#3190,#3191));
#1442=EDGE_LOOP('',(#3192,#3193));
#1443=EDGE_LOOP('',(#3194,#3195));
#1444=EDGE_LOOP('',(#3196,#3197));
#1445=EDGE_LOOP('',(#3198,#3199));
#1446=EDGE_LOOP('',(#3200,#3201));
#1447=EDGE_LOOP('',(#3202,#3203));
#1448=EDGE_LOOP('',(#3204,#3205,#3206,#3207));
#1449=EDGE_LOOP('',(#3208,#3209,#3210,#3211,#3212,#3213,#3214,#3215,#3216,
#3217,#3218,#3219,#3220,#3221,#3222,#3223,#3224,#3225,#3226,#3227));
#1450=EDGE_LOOP('',(#3228,#3229,#3230,#3231));
#1451=EDGE_LOOP('',(#3232,#3233,#3234,#3235));
#1452=EDGE_LOOP('',(#3236,#3237,#3238,#3239));
#1453=EDGE_LOOP('',(#3240,#3241,#3242,#3243));
#1454=EDGE_LOOP('',(#3244,#3245,#3246,#3247));
#1455=EDGE_LOOP('',(#3248,#3249,#3250,#3251,#3252,#3253));
#1456=EDGE_LOOP('',(#3254,#3255,#3256,#3257));
#1457=EDGE_LOOP('',(#3258,#3259,#3260,#3261));
#1458=EDGE_LOOP('',(#3262,#3263,#3264,#3265));
#1459=EDGE_LOOP('',(#3266,#3267,#3268,#3269));
#1460=EDGE_LOOP('',(#3270,#3271,#3272,#3273));
#1461=EDGE_LOOP('',(#3274,#3275,#3276,#3277));
#1462=EDGE_LOOP('',(#3278,#3279,#3280,#3281,#3282,#3283,#3284,#3285,#3286,
#3287,#3288,#3289,#3290,#3291,#3292,#3293,#3294,#3295,#3296,#3297));
#1463=EDGE_LOOP('',(#3298,#3299,#3300,#3301));
#1464=EDGE_LOOP('',(#3302,#3303,#3304,#3305));
#1465=EDGE_LOOP('',(#3306));
#1466=EDGE_LOOP('',(#3307));
#1467=EDGE_LOOP('',(#3308,#3309,#3310,#3311));
#1468=EDGE_LOOP('',(#3312));
#1469=EDGE_LOOP('',(#3313));
#1470=EDGE_LOOP('',(#3314,#3315,#3316,#3317));
#1471=EDGE_LOOP('',(#3318));
#1472=EDGE_LOOP('',(#3319));
#1473=EDGE_LOOP('',(#3320,#3321,#3322,#3323));
#1474=EDGE_LOOP('',(#3324));
#1475=EDGE_LOOP('',(#3325));
#1476=EDGE_LOOP('',(#3326,#3327,#3328,#3329));
#1477=EDGE_LOOP('',(#3330));
#1478=EDGE_LOOP('',(#3331));
#1479=EDGE_LOOP('',(#3332,#3333,#3334,#3335));
#1480=EDGE_LOOP('',(#3336,#3337,#3338,#3339));
#1481=EDGE_LOOP('',(#3340,#3341,#3342,#3343));
#1482=EDGE_LOOP('',(#3344,#3345,#3346,#3347));
#1483=EDGE_LOOP('',(#3348,#3349,#3350,#3351));
#1484=EDGE_LOOP('',(#3352,#3353,#3354,#3355));
#1485=EDGE_LOOP('',(#3356));
#1486=EDGE_LOOP('',(#3357));
#1487=EDGE_LOOP('',(#3358,#3359,#3360,#3361));
#1488=EDGE_LOOP('',(#3362,#3363,#3364,#3365));
#1489=EDGE_LOOP('',(#3366));
#1490=EDGE_LOOP('',(#3367));
#1491=EDGE_LOOP('',(#3368));
#1492=EDGE_LOOP('',(#3369));
#1493=EDGE_LOOP('',(#3370));
#1494=EDGE_LOOP('',(#3371));
#1495=EDGE_LOOP('',(#3372));
#1496=EDGE_LOOP('',(#3373));
#1497=EDGE_LOOP('',(#3374));
#1498=EDGE_LOOP('',(#3375));
#1499=EDGE_LOOP('',(#3376));
#1500=EDGE_LOOP('',(#3377));
#1501=EDGE_LOOP('',(#3378,#3379,#3380,#3381));
#1502=EDGE_LOOP('',(#3382,#3383,#3384,#3385));
#1503=EDGE_LOOP('',(#3386,#3387,#3388,#3389));
#1504=EDGE_LOOP('',(#3390,#3391,#3392,#3393));
#1505=EDGE_LOOP('',(#3394,#3395,#3396,#3397));
#1506=EDGE_LOOP('',(#3398,#3399,#3400,#3401));
#1507=EDGE_LOOP('',(#3402,#3403,#3404,#3405,#3406,#3407));
#1508=EDGE_LOOP('',(#3408,#3409,#3410,#3411,#3412,#3413));
#1509=EDGE_LOOP('',(#3414));
#1510=EDGE_LOOP('',(#3415));
#1511=EDGE_LOOP('',(#3416,#3417,#3418,#3419));
#1512=EDGE_LOOP('',(#3420,#3421,#3422,#3423));
#1513=EDGE_LOOP('',(#3424,#3425,#3426,#3427));
#1514=EDGE_LOOP('',(#3428));
#1515=EDGE_LOOP('',(#3429));
#1516=EDGE_LOOP('',(#3430,#3431,#3432,#3433));
#1517=EDGE_LOOP('',(#3434,#3435,#3436,#3437));
#1518=EDGE_LOOP('',(#3438));
#1519=EDGE_LOOP('',(#3439));
#1520=EDGE_LOOP('',(#3440));
#1521=EDGE_LOOP('',(#3441));
#1522=EDGE_LOOP('',(#3442,#3443,#3444,#3445));
#1523=EDGE_LOOP('',(#3446,#3447,#3448,#3449,#3450,#3451));
#1524=EDGE_LOOP('',(#3452,#3453,#3454,#3455));
#1525=EDGE_LOOP('',(#3456));
#1526=EDGE_LOOP('',(#3457,#3458,#3459,#3460));
#1527=EDGE_LOOP('',(#3461,#3462,#3463,#3464,#3465));
#1528=EDGE_LOOP('',(#3466,#3467,#3468,#3469));
#1529=EDGE_LOOP('',(#3470,#3471,#3472,#3473));
#1530=EDGE_LOOP('',(#3474,#3475,#3476,#3477,#3478,#3479,#3480,#3481));
#1531=EDGE_LOOP('',(#3482,#3483,#3484,#3485));
#1532=EDGE_LOOP('',(#3486,#3487,#3488,#3489,#3490,#3491,#3492,#3493));
#1533=EDGE_LOOP('',(#3494,#3495,#3496,#3497));
#1534=EDGE_LOOP('',(#3498,#3499,#3500,#3501));
#1535=EDGE_LOOP('',(#3502,#3503,#3504,#3505));
#1536=EDGE_LOOP('',(#3506,#3507,#3508,#3509));
#1537=EDGE_LOOP('',(#3510,#3511,#3512,#3513));
#1538=EDGE_LOOP('',(#3514));
#1539=EDGE_LOOP('',(#3515));
#1540=EDGE_LOOP('',(#3516));
#1541=EDGE_LOOP('',(#3517));
#1542=EDGE_LOOP('',(#3518,#3519,#3520,#3521));
#1543=EDGE_LOOP('',(#3522,#3523,#3524,#3525));
#1544=EDGE_LOOP('',(#3526,#3527,#3528,#3529));
#1545=EDGE_LOOP('',(#3530,#3531,#3532,#3533));
#1546=EDGE_LOOP('',(#3534,#3535,#3536,#3537));
#1547=EDGE_LOOP('',(#3538,#3539,#3540,#3541));
#1548=EDGE_LOOP('',(#3542,#3543,#3544,#3545));
#1549=EDGE_LOOP('',(#3546,#3547,#3548,#3549,#3550,#3551));
#1550=EDGE_LOOP('',(#3552));
#1551=EDGE_LOOP('',(#3553,#3554,#3555,#3556,#3557,#3558));
#1552=EDGE_LOOP('',(#3559));
#1553=CIRCLE('',#4223,0.9);
#1554=CIRCLE('',#4224,3.25);
#1555=CIRCLE('',#4225,0.9);
#1556=CIRCLE('',#4226,3.25);
#1557=CIRCLE('',#4227,0.9);
#1558=CIRCLE('',#4228,3.25);
#1559=CIRCLE('',#4229,0.9);
#1560=CIRCLE('',#4230,3.25);
#1561=CIRCLE('',#4231,1.2);
#1562=CIRCLE('',#4233,3.25);
#1563=CIRCLE('',#4235,3.25);
#1564=CIRCLE('',#4237,3.25);
#1565=CIRCLE('',#4239,1.2);
#1566=CIRCLE('',#4241,3.25);
#1567=CIRCLE('',#4243,0.9);
#1568=CIRCLE('',#4244,0.9);
#1569=CIRCLE('',#4245,0.9);
#1570=CIRCLE('',#4247,0.9);
#1571=CIRCLE('',#4248,0.9);
#1572=CIRCLE('',#4249,0.9);
#1573=CIRCLE('',#4251,0.9);
#1574=CIRCLE('',#4252,0.9);
#1575=CIRCLE('',#4253,0.9);
#1576=CIRCLE('',#4255,1.);
#1577=CIRCLE('',#4257,0.9);
#1578=CIRCLE('',#4258,0.9);
#1579=CIRCLE('',#4259,0.9);
#1580=CIRCLE('',#4261,0.425);
#1581=CIRCLE('',#4262,0.425);
#1582=CIRCLE('',#4264,0.425);
#1583=CIRCLE('',#4265,0.425);
#1584=CIRCLE('',#4267,0.425);
#1585=CIRCLE('',#4268,0.425);
#1586=CIRCLE('',#4270,1.);
#1587=CIRCLE('',#4283,1.1);
#1588=CIRCLE('',#4284,1.1);
#1589=CIRCLE('',#4286,0.425);
#1590=CIRCLE('',#4287,0.425);
#1591=CIRCLE('',#4289,0.425);
#1592=CIRCLE('',#4290,0.425);
#1593=CIRCLE('',#4299,0.425);
#1594=CIRCLE('',#4300,0.425);
#1595=CIRCLE('',#4302,1.);
#1596=CIRCLE('',#4303,1.);
#1597=CIRCLE('',#4308,0.34);
#1598=CIRCLE('',#4309,0.34);
#1599=CIRCLE('',#4312,1.5);
#1600=CIRCLE('',#4313,1.);
#1601=CIRCLE('',#4315,1.5);
#1602=CIRCLE('',#4318,1.);
#1603=CIRCLE('',#4322,0.425);
#1604=CIRCLE('',#4323,0.425);
#1605=CIRCLE('',#4325,1.5);
#1606=CIRCLE('',#4326,1.5);
#1607=CIRCLE('',#4331,1.005);
#1608=CIRCLE('',#4332,1.005);
#1609=CIRCLE('',#4334,1.4);
#1610=CIRCLE('',#4335,1.4);
#1611=CIRCLE('',#4340,0.81);
#1612=CIRCLE('',#4341,0.81);
#1613=CIRCLE('',#4343,1.1);
#1614=CIRCLE('',#4344,1.1);
#1615=CIRCLE('',#4349,1.005);
#1616=CIRCLE('',#4350,1.005);
#1617=CIRCLE('',#4352,1.4);
#1618=CIRCLE('',#4353,1.4);
#1619=CIRCLE('',#4366,0.4);
#1620=CIRCLE('',#4367,0.3933);
#1621=CIRCLE('',#4369,0.4);
#1622=CIRCLE('',#4372,0.6);
#1623=CIRCLE('',#4374,0.65);
#1624=CIRCLE('',#4376,0.65);
#1625=CIRCLE('',#4378,0.62);
#1626=CIRCLE('',#4380,0.42);
#1627=CIRCLE('',#4382,0.3933);
#1628=CIRCLE('',#4386,0.42);
#1629=CIRCLE('',#4387,0.42);
#1630=CIRCLE('',#4389,0.8);
#1631=CIRCLE('',#4390,0.8);
#1632=CIRCLE('',#4395,0.6175);
#1633=CIRCLE('',#4397,0.6175);
#1634=CIRCLE('',#4402,0.338975);
#1635=CIRCLE('',#4403,0.338975);
#1636=CIRCLE('',#4411,0.6);
#1637=CIRCLE('',#4413,0.65);
#1638=CIRCLE('',#4415,0.65);
#1639=CIRCLE('',#4417,0.62);
#1640=CIRCLE('',#4419,0.42);
#1641=CIRCLE('',#4421,0.3933);
#1642=CIRCLE('',#4423,0.3933);
#1643=CIRCLE('',#4425,0.32);
#1644=CIRCLE('',#4461,0.165);
#1645=CIRCLE('',#4462,0.165);
#1646=CIRCLE('',#4464,0.165);
#1647=CIRCLE('',#4465,0.165);
#1648=CIRCLE('',#4467,0.165);
#1649=CIRCLE('',#4468,0.165);
#1650=CIRCLE('',#4470,0.165);
#1651=CIRCLE('',#4471,0.165);
#1652=CIRCLE('',#4473,4.4);
#1653=CIRCLE('',#4474,5.);
#1654=CIRCLE('',#4476,5.);
#1655=CIRCLE('',#4478,5.);
#1656=CIRCLE('',#4480,3.);
#1657=CIRCLE('',#4482,5.);
#1658=CIRCLE('',#4483,3.);
#1659=CIRCLE('',#4486,3.);
#1660=CIRCLE('',#4488,2.35);
#1661=CIRCLE('',#4489,2.35);
#1662=CIRCLE('',#4491,3.);
#1663=CIRCLE('',#4496,1.9);
#1664=CIRCLE('',#4497,1.9);
#1665=CIRCLE('',#4499,2.34);
#1666=CIRCLE('',#4500,2.34);
#1667=CIRCLE('',#4506,1.63531);
#1668=CIRCLE('',#4507,1.63531);
#1669=CIRCLE('',#4508,0.412776);
#1670=CIRCLE('',#4509,1.63531);
#1671=CIRCLE('',#4510,1.63531);
#1672=CIRCLE('',#4512,1.63531);
#1673=CIRCLE('',#4514,1.);
#1674=CIRCLE('',#4515,1.);
#1675=CIRCLE('',#4517,1.1);
#1676=CIRCLE('',#4520,1.63531);
#1677=CIRCLE('',#4522,1.1);
#1678=CIRCLE('',#4526,1.71469);
#1679=CIRCLE('',#4527,1.71469);
#1680=CIRCLE('',#4528,0.412776);
#1681=CIRCLE('',#4529,1.71469);
#1682=CIRCLE('',#4530,1.71469);
#1683=CIRCLE('',#4532,1.71469);
#1684=CIRCLE('',#4534,2.25);
#1685=CIRCLE('',#4535,1.71469);
#1686=CIRCLE('',#4537,2.35);
#1687=CIRCLE('',#4539,2.35);
#1688=CIRCLE('',#4541,2.25);
#1689=CIRCLE('',#4546,0.3969);
#1690=CIRCLE('',#4548,0.3969);
#1691=CIRCLE('',#4550,0.3969);
#1692=CIRCLE('',#4552,0.3969);
#1693=CIRCLE('',#4554,0.3969);
#1694=CIRCLE('',#4556,0.3969);
#1695=CIRCLE('',#4558,0.3969);
#1696=CIRCLE('',#4560,0.3969);
#1697=CIRCLE('',#4563,0.405071403305639);
#1698=CIRCLE('',#4564,0.405071403305639);
#1699=CIRCLE('',#4566,1.706752);
#1700=CIRCLE('',#4567,1.706752);
#1701=CIRCLE('',#4568,1.706752);
#1702=CIRCLE('',#4569,1.706752);
#1703=CIRCLE('',#4570,1.706752);
#1704=CIRCLE('',#4571,1.706752);
#1705=CIRCLE('',#4572,1.706752);
#1706=CIRCLE('',#4573,1.706752);
#1707=CIRCLE('',#4574,1.706752);
#1708=CIRCLE('',#4576,1.643248);
#1709=CIRCLE('',#4577,0.405071403305639);
#1710=CIRCLE('',#4579,0.405071403305639);
#1711=CIRCLE('',#4581,1.643248);
#1712=CIRCLE('',#4582,0.405071403305639);
#1713=CIRCLE('',#4584,0.405071403305639);
#1714=CIRCLE('',#4586,1.643248);
#1715=CIRCLE('',#4587,0.405071403305639);
#1716=CIRCLE('',#4589,0.405071403305639);
#1717=CIRCLE('',#4591,1.643248);
#1718=CIRCLE('',#4592,0.405071403305639);
#1719=CIRCLE('',#4594,0.405071403305639);
#1720=CIRCLE('',#4596,1.643248);
#1721=CIRCLE('',#4597,0.405071403305639);
#1722=CIRCLE('',#4599,0.405071403305639);
#1723=CIRCLE('',#4601,1.643248);
#1724=CIRCLE('',#4602,0.405071403305639);
#1725=CIRCLE('',#4604,0.405071403305639);
#1726=CIRCLE('',#4606,1.643248);
#1727=CIRCLE('',#4607,1.643248);
#1728=CIRCLE('',#4608,1.643248);
#1729=CIRCLE('',#4610,0.405071403305639);
#1730=CIRCLE('',#4612,0.405071403305639);
#1731=CIRCLE('',#4617,1.70469);
#1732=CIRCLE('',#4618,1.65031);
#1733=CIRCLE('',#4620,1.70469);
#1734=CIRCLE('',#4622,1.65031);
#1735=CIRCLE('',#4625,1.70469);
#1736=CIRCLE('',#4626,1.65031);
#1737=CIRCLE('',#4628,1.70469);
#1738=CIRCLE('',#4630,1.65031);
#1739=CIRCLE('',#4639,0.225);
#1740=CIRCLE('',#4640,0.225);
#1741=CIRCLE('',#4642,0.225);
#1742=CIRCLE('',#4643,0.225);
#1743=CIRCLE('',#4645,0.225);
#1744=CIRCLE('',#4646,0.225);
#1745=CIRCLE('',#4648,0.225);
#1746=CIRCLE('',#4649,0.225);
#1747=CIRCLE('',#4651,2.34);
#1748=CIRCLE('',#4652,2.34);
#1749=CIRCLE('',#4654,1.9);
#1750=CIRCLE('',#4656,1.9);
#1751=CIRCLE('',#4658,3.);
#1752=CIRCLE('',#4659,3.);
#1753=CIRCLE('',#4672,0.1954);
#1754=CIRCLE('',#4674,0.3);
#1755=CIRCLE('',#4676,0.35);
#1756=CIRCLE('',#4678,0.35);
#1757=CIRCLE('',#4680,0.32);
#1758=CIRCLE('',#4682,0.22);
#1759=CIRCLE('',#4684,0.1954);
#1760=CIRCLE('',#4703,1.3);
#1761=CIRCLE('',#4704,0.8);
#1762=CIRCLE('',#4706,1.3);
#1763=CIRCLE('',#4707,0.8);
#1764=CIRCLE('',#4710,0.8);
#1765=CIRCLE('',#4711,0.8);
#1766=CIRCLE('',#4712,0.8);
#1767=CIRCLE('',#4714,0.8);
#1768=CIRCLE('',#4721,2.);
#1769=CIRCLE('',#4722,3.5);
#1770=CIRCLE('',#4724,2.);
#1771=CIRCLE('',#4726,3.5);
#1772=CIRCLE('',#4732,0.81);
#1773=CIRCLE('',#4733,0.81);
#1774=CIRCLE('',#4735,1.5);
#1775=CIRCLE('',#4736,1.5);
#1776=CIRCLE('',#4741,0.7);
#1777=CIRCLE('',#4742,0.7);
#1778=VERTEX_POINT('',#6067);
#1779=VERTEX_POINT('',#6068);
#1780=VERTEX_POINT('',#6070);
#1781=VERTEX_POINT('',#6072);
#1782=VERTEX_POINT('',#6074);
#1783=VERTEX_POINT('',#6076);
#1784=VERTEX_POINT('',#6078);
#1785=VERTEX_POINT('',#6080);
#1786=VERTEX_POINT('',#6083);
#1787=VERTEX_POINT('',#6086);
#1788=VERTEX_POINT('',#6088);
#1789=VERTEX_POINT('',#6092);
#1790=VERTEX_POINT('',#6094);
#1791=VERTEX_POINT('',#6098);
#1792=VERTEX_POINT('',#6100);
#1793=VERTEX_POINT('',#6104);
#1794=VERTEX_POINT('',#6108);
#1795=VERTEX_POINT('',#6110);
#1796=VERTEX_POINT('',#6114);
#1797=VERTEX_POINT('',#6116);
#1798=VERTEX_POINT('',#6121);
#1799=VERTEX_POINT('',#6123);
#1800=VERTEX_POINT('',#6128);
#1801=VERTEX_POINT('',#6130);
#1802=VERTEX_POINT('',#6135);
#1803=VERTEX_POINT('',#6138);
#1804=VERTEX_POINT('',#6140);
#1805=VERTEX_POINT('',#6145);
#1806=VERTEX_POINT('',#6147);
#1807=VERTEX_POINT('',#6151);
#1808=VERTEX_POINT('',#6153);
#1809=VERTEX_POINT('',#6157);
#1810=VERTEX_POINT('',#6159);
#1811=VERTEX_POINT('',#6163);
#1812=VERTEX_POINT('',#6167);
#1813=VERTEX_POINT('',#6168);
#1814=VERTEX_POINT('',#6170);
#1815=VERTEX_POINT('',#6172);
#1816=VERTEX_POINT('',#6176);
#1817=VERTEX_POINT('',#6178);
#1818=VERTEX_POINT('',#6182);
#1819=VERTEX_POINT('',#6184);
#1820=VERTEX_POINT('',#6188);
#1821=VERTEX_POINT('',#6190);
#1822=VERTEX_POINT('',#6194);
#1823=VERTEX_POINT('',#6196);
#1824=VERTEX_POINT('',#6200);
#1825=VERTEX_POINT('',#6202);
#1826=VERTEX_POINT('',#6206);
#1827=VERTEX_POINT('',#6208);
#1828=VERTEX_POINT('',#6218);
#1829=VERTEX_POINT('',#6220);
#1830=VERTEX_POINT('',#6224);
#1831=VERTEX_POINT('',#6226);
#1832=VERTEX_POINT('',#6230);
#1833=VERTEX_POINT('',#6232);
#1834=VERTEX_POINT('',#6236);
#1835=VERTEX_POINT('',#6237);
#1836=VERTEX_POINT('',#6239);
#1837=VERTEX_POINT('',#6241);
#1838=VERTEX_POINT('',#6245);
#1839=VERTEX_POINT('',#6247);
#1840=VERTEX_POINT('',#6251);
#1841=VERTEX_POINT('',#6253);
#1842=VERTEX_POINT('',#6263);
#1843=VERTEX_POINT('',#6265);
#1844=VERTEX_POINT('',#6269);
#1845=VERTEX_POINT('',#6271);
#1846=VERTEX_POINT('',#6278);
#1847=VERTEX_POINT('',#6280);
#1848=VERTEX_POINT('',#6285);
#1849=VERTEX_POINT('',#6287);
#1850=VERTEX_POINT('',#6290);
#1851=VERTEX_POINT('',#6295);
#1852=VERTEX_POINT('',#6301);
#1853=VERTEX_POINT('',#6303);
#1854=VERTEX_POINT('',#6307);
#1855=VERTEX_POINT('',#6309);
#1856=VERTEX_POINT('',#6316);
#1857=VERTEX_POINT('',#6318);
#1858=VERTEX_POINT('',#6322);
#1859=VERTEX_POINT('',#6324);
#1860=VERTEX_POINT('',#6331);
#1861=VERTEX_POINT('',#6333);
#1862=VERTEX_POINT('',#6337);
#1863=VERTEX_POINT('',#6339);
#1864=VERTEX_POINT('',#6346);
#1865=VERTEX_POINT('',#6348);
#1866=VERTEX_POINT('',#6352);
#1867=VERTEX_POINT('',#6354);
#1868=VERTEX_POINT('',#6361);
#1869=VERTEX_POINT('',#6362);
#1870=VERTEX_POINT('',#6364);
#1871=VERTEX_POINT('',#6366);
#1872=VERTEX_POINT('',#6370);
#1873=VERTEX_POINT('',#6372);
#1874=VERTEX_POINT('',#6376);
#1875=VERTEX_POINT('',#6378);
#1876=VERTEX_POINT('',#6382);
#1877=VERTEX_POINT('',#6384);
#1878=VERTEX_POINT('',#6388);
#1879=VERTEX_POINT('',#6390);
#1880=VERTEX_POINT('',#6399);
#1881=VERTEX_POINT('',#6401);
#1882=VERTEX_POINT('',#6404);
#1883=VERTEX_POINT('',#6409);
#1884=VERTEX_POINT('',#6412);
#1885=VERTEX_POINT('',#6416);
#1886=VERTEX_POINT('',#6420);
#1887=VERTEX_POINT('',#6424);
#1888=VERTEX_POINT('',#6427);
#1889=VERTEX_POINT('',#6434);
#1890=VERTEX_POINT('',#6436);
#1891=VERTEX_POINT('',#6440);
#1892=VERTEX_POINT('',#6442);
#1893=VERTEX_POINT('',#6449);
#1894=VERTEX_POINT('',#6450);
#1895=VERTEX_POINT('',#6454);
#1896=VERTEX_POINT('',#6458);
#1897=VERTEX_POINT('',#6461);
#1898=VERTEX_POINT('',#6465);
#1899=VERTEX_POINT('',#6469);
#1900=VERTEX_POINT('',#6477);
#1901=VERTEX_POINT('',#6479);
#1902=VERTEX_POINT('',#6481);
#1903=VERTEX_POINT('',#6485);
#1904=VERTEX_POINT('',#6489);
#1905=VERTEX_POINT('',#6493);
#1906=VERTEX_POINT('',#6497);
#1907=VERTEX_POINT('',#6512);
#1908=VERTEX_POINT('',#6514);
#1909=VERTEX_POINT('',#6526);
#1910=VERTEX_POINT('',#6529);
#1911=VERTEX_POINT('',#6533);
#1912=VERTEX_POINT('',#6537);
#1913=VERTEX_POINT('',#6541);
#1914=VERTEX_POINT('',#6544);
#1915=VERTEX_POINT('',#6548);
#1916=VERTEX_POINT('',#6552);
#1917=VERTEX_POINT('',#6557);
#1918=VERTEX_POINT('',#6558);
#1919=VERTEX_POINT('',#6560);
#1920=VERTEX_POINT('',#6562);
#1921=VERTEX_POINT('',#6566);
#1922=VERTEX_POINT('',#6568);
#1923=VERTEX_POINT('',#6572);
#1924=VERTEX_POINT('',#6574);
#1925=VERTEX_POINT('',#6578);
#1926=VERTEX_POINT('',#6580);
#1927=VERTEX_POINT('',#6584);
#1928=VERTEX_POINT('',#6586);
#1929=VERTEX_POINT('',#6620);
#1930=VERTEX_POINT('',#6622);
#1931=VERTEX_POINT('',#6626);
#1932=VERTEX_POINT('',#6628);
#1933=VERTEX_POINT('',#6632);
#1934=VERTEX_POINT('',#6634);
#1935=VERTEX_POINT('',#6638);
#1936=VERTEX_POINT('',#6640);
#1937=VERTEX_POINT('',#6644);
#1938=VERTEX_POINT('',#6646);
#1939=VERTEX_POINT('',#6650);
#1940=VERTEX_POINT('',#6654);
#1941=VERTEX_POINT('',#6658);
#1942=VERTEX_POINT('',#6661);
#1943=VERTEX_POINT('',#6663);
#1944=VERTEX_POINT('',#6668);
#1945=VERTEX_POINT('',#6672);
#1946=VERTEX_POINT('',#6674);
#1947=VERTEX_POINT('',#6678);
#1948=VERTEX_POINT('',#6685);
#1949=VERTEX_POINT('',#6687);
#1950=VERTEX_POINT('',#6691);
#1951=VERTEX_POINT('',#6693);
#1952=VERTEX_POINT('',#6701);
#1953=VERTEX_POINT('',#6702);
#1954=VERTEX_POINT('',#6705);
#1955=VERTEX_POINT('',#6707);
#1956=VERTEX_POINT('',#6711);
#1957=VERTEX_POINT('',#6715);
#1958=VERTEX_POINT('',#6717);
#1959=VERTEX_POINT('',#6721);
#1960=VERTEX_POINT('',#6726);
#1961=VERTEX_POINT('',#6730);
#1962=VERTEX_POINT('',#6736);
#1963=VERTEX_POINT('',#6737);
#1964=VERTEX_POINT('',#6740);
#1965=VERTEX_POINT('',#6742);
#1966=VERTEX_POINT('',#6746);
#1967=VERTEX_POINT('',#6750);
#1968=VERTEX_POINT('',#6752);
#1969=VERTEX_POINT('',#6755);
#1970=VERTEX_POINT('',#6759);
#1971=VERTEX_POINT('',#6763);
#1972=VERTEX_POINT('',#6771);
#1973=VERTEX_POINT('',#6772);
#1974=VERTEX_POINT('',#6775);
#1975=VERTEX_POINT('',#6776);
#1976=VERTEX_POINT('',#6779);
#1977=VERTEX_POINT('',#6780);
#1978=VERTEX_POINT('',#6783);
#1979=VERTEX_POINT('',#6784);
#1980=VERTEX_POINT('',#6787);
#1981=VERTEX_POINT('',#6788);
#1982=VERTEX_POINT('',#6791);
#1983=VERTEX_POINT('',#6792);
#1984=VERTEX_POINT('',#6795);
#1985=VERTEX_POINT('',#6796);
#1986=VERTEX_POINT('',#6799);
#1987=VERTEX_POINT('',#6800);
#1988=VERTEX_POINT('',#6804);
#1989=VERTEX_POINT('',#6805);
#1990=VERTEX_POINT('',#6828);
#1991=VERTEX_POINT('',#6830);
#1992=VERTEX_POINT('',#6855);
#1993=VERTEX_POINT('',#6857);
#1994=VERTEX_POINT('',#6880);
#1995=VERTEX_POINT('',#6882);
#1996=VERTEX_POINT('',#6905);
#1997=VERTEX_POINT('',#6907);
#1998=VERTEX_POINT('',#6920);
#1999=VERTEX_POINT('',#6923);
#2000=VERTEX_POINT('',#6936);
#2001=VERTEX_POINT('',#6938);
#2002=VERTEX_POINT('',#6961);
#2003=VERTEX_POINT('',#6963);
#2004=VERTEX_POINT('',#6986);
#2005=VERTEX_POINT('',#6988);
#2006=VERTEX_POINT('',#7011);
#2007=VERTEX_POINT('',#7013);
#2008=VERTEX_POINT('',#7038);
#2009=VERTEX_POINT('',#7042);
#2010=VERTEX_POINT('',#7067);
#2011=VERTEX_POINT('',#7071);
#2012=VERTEX_POINT('',#7096);
#2013=VERTEX_POINT('',#7100);
#2014=VERTEX_POINT('',#7101);
#2015=VERTEX_POINT('',#7128);
#2016=VERTEX_POINT('',#7132);
#2017=VERTEX_POINT('',#7157);
#2018=VERTEX_POINT('',#7161);
#2019=VERTEX_POINT('',#7186);
#2020=VERTEX_POINT('',#7190);
#2021=VERTEX_POINT('',#7215);
#2022=VERTEX_POINT('',#7218);
#2023=VERTEX_POINT('',#7220);
#2024=VERTEX_POINT('',#7252);
#2025=VERTEX_POINT('',#7254);
#2026=VERTEX_POINT('',#7257);
#2027=VERTEX_POINT('',#7261);
#2028=VERTEX_POINT('',#7266);
#2029=VERTEX_POINT('',#7268);
#2030=VERTEX_POINT('',#7271);
#2031=VERTEX_POINT('',#7275);
#2032=VERTEX_POINT('',#7286);
#2033=VERTEX_POINT('',#7288);
#2034=VERTEX_POINT('',#7292);
#2035=VERTEX_POINT('',#7294);
#2036=VERTEX_POINT('',#7298);
#2037=VERTEX_POINT('',#7300);
#2038=VERTEX_POINT('',#7304);
#2039=VERTEX_POINT('',#7306);
#2040=VERTEX_POINT('',#7310);
#2041=VERTEX_POINT('',#7312);
#2042=VERTEX_POINT('',#7316);
#2043=VERTEX_POINT('',#7319);
#2044=VERTEX_POINT('',#7323);
#2045=VERTEX_POINT('',#7325);
#2046=VERTEX_POINT('',#7332);
#2047=VERTEX_POINT('',#7333);
#2048=VERTEX_POINT('',#7335);
#2049=VERTEX_POINT('',#7337);
#2050=VERTEX_POINT('',#7341);
#2051=VERTEX_POINT('',#7343);
#2052=VERTEX_POINT('',#7347);
#2053=VERTEX_POINT('',#7349);
#2054=VERTEX_POINT('',#7353);
#2055=VERTEX_POINT('',#7355);
#2056=VERTEX_POINT('',#7359);
#2057=VERTEX_POINT('',#7361);
#2058=VERTEX_POINT('',#7370);
#2059=VERTEX_POINT('',#7373);
#2060=VERTEX_POINT('',#7376);
#2061=VERTEX_POINT('',#7380);
#2062=VERTEX_POINT('',#7384);
#2063=VERTEX_POINT('',#7388);
#2064=VERTEX_POINT('',#7391);
#2065=VERTEX_POINT('',#7413);
#2066=VERTEX_POINT('',#7415);
#2067=VERTEX_POINT('',#7418);
#2068=VERTEX_POINT('',#7420);
#2069=VERTEX_POINT('',#7425);
#2070=VERTEX_POINT('',#7427);
#2071=VERTEX_POINT('',#7429);
#2072=VERTEX_POINT('',#7433);
#2073=VERTEX_POINT('',#7438);
#2074=VERTEX_POINT('',#7440);
#2075=VERTEX_POINT('',#7444);
#2076=VERTEX_POINT('',#7446);
#2077=VERTEX_POINT('',#7450);
#2078=VERTEX_POINT('',#7451);
#2079=VERTEX_POINT('',#7456);
#2080=VERTEX_POINT('',#7457);
#2081=VERTEX_POINT('',#7459);
#2082=VERTEX_POINT('',#7461);
#2083=VERTEX_POINT('',#7466);
#2084=VERTEX_POINT('',#7468);
#2085=VERTEX_POINT('',#7472);
#2086=VERTEX_POINT('',#7477);
#2087=VERTEX_POINT('',#7486);
#2088=VERTEX_POINT('',#7488);
#2089=VERTEX_POINT('',#7492);
#2090=VERTEX_POINT('',#7494);
#2091=VERTEX_POINT('',#7501);
#2092=VERTEX_POINT('',#7503);
#2093=VERTEX_POINT('',#7507);
#2094=VERTEX_POINT('',#7508);
#2095=VERTEX_POINT('',#7510);
#2096=VERTEX_POINT('',#7512);
#2097=VERTEX_POINT('',#7516);
#2098=VERTEX_POINT('',#7518);
#2099=VERTEX_POINT('',#7522);
#2100=VERTEX_POINT('',#7524);
#2101=VERTEX_POINT('',#7528);
#2102=VERTEX_POINT('',#7530);
#2103=VERTEX_POINT('',#7534);
#2104=VERTEX_POINT('',#7536);
#2105=EDGE_CURVE('',#1778,#1779,#1553,.T.);
#2106=EDGE_CURVE('',#1778,#1780,#1554,.T.);
#2107=EDGE_CURVE('',#1781,#1780,#1555,.T.);
#2108=EDGE_CURVE('',#1781,#1782,#1556,.T.);
#2109=EDGE_CURVE('',#1783,#1782,#1557,.T.);
#2110=EDGE_CURVE('',#1783,#1784,#1558,.T.);
#2111=EDGE_CURVE('',#1785,#1784,#1559,.T.);
#2112=EDGE_CURVE('',#1785,#1779,#1560,.T.);
#2113=EDGE_CURVE('',#1786,#1786,#1561,.T.);
#2114=EDGE_CURVE('',#1784,#1787,#384,.T.);
#2115=EDGE_CURVE('',#1788,#1783,#385,.T.);
#2116=EDGE_CURVE('',#1787,#1788,#1562,.T.);
#2117=EDGE_CURVE('',#1789,#1781,#386,.T.);
#2118=EDGE_CURVE('',#1790,#1789,#1563,.T.);
#2119=EDGE_CURVE('',#1782,#1790,#387,.T.);
#2120=EDGE_CURVE('',#1779,#1791,#388,.T.);
#2121=EDGE_CURVE('',#1792,#1785,#389,.T.);
#2122=EDGE_CURVE('',#1791,#1792,#1564,.T.);
#2123=EDGE_CURVE('',#1786,#1793,#390,.T.);
#2124=EDGE_CURVE('',#1793,#1793,#1565,.T.);
#2125=EDGE_CURVE('',#1794,#1778,#391,.T.);
#2126=EDGE_CURVE('',#1795,#1794,#1566,.T.);
#2127=EDGE_CURVE('',#1780,#1795,#392,.T.);
#2128=EDGE_CURVE('',#1796,#1796,#1567,.T.);
#2129=EDGE_CURVE('',#1796,#1797,#393,.T.);
#2130=EDGE_CURVE('',#1794,#1797,#1568,.T.);
#2131=EDGE_CURVE('',#1797,#1791,#1569,.T.);
#2132=EDGE_CURVE('',#1798,#1798,#1570,.T.);
#2133=EDGE_CURVE('',#1798,#1799,#394,.T.);
#2134=EDGE_CURVE('',#1792,#1799,#1571,.T.);
#2135=EDGE_CURVE('',#1799,#1787,#1572,.T.);
#2136=EDGE_CURVE('',#1800,#1800,#1573,.T.);
#2137=EDGE_CURVE('',#1800,#1801,#395,.T.);
#2138=EDGE_CURVE('',#1788,#1801,#1574,.T.);
#2139=EDGE_CURVE('',#1801,#1790,#1575,.T.);
#2140=EDGE_CURVE('',#1802,#1802,#1576,.T.);
#2141=EDGE_CURVE('',#1803,#1803,#1577,.T.);
#2142=EDGE_CURVE('',#1803,#1804,#396,.T.);
#2143=EDGE_CURVE('',#1789,#1804,#1578,.T.);
#2144=EDGE_CURVE('',#1804,#1795,#1579,.T.);
#2145=EDGE_CURVE('',#1805,#1805,#1580,.T.);
#2146=EDGE_CURVE('',#1805,#1806,#397,.T.);
#2147=EDGE_CURVE('',#1806,#1806,#1581,.T.);
#2148=EDGE_CURVE('',#1807,#1807,#1582,.T.);
#2149=EDGE_CURVE('',#1807,#1808,#398,.T.);
#2150=EDGE_CURVE('',#1808,#1808,#1583,.T.);
#2151=EDGE_CURVE('',#1809,#1809,#1584,.T.);
#2152=EDGE_CURVE('',#1809,#1810,#399,.T.);
#2153=EDGE_CURVE('',#1810,#1810,#1585,.T.);
#2154=EDGE_CURVE('',#1811,#1811,#1586,.T.);
#2155=EDGE_CURVE('',#1811,#1802,#400,.T.);
#2156=EDGE_CURVE('',#1812,#1813,#401,.T.);
#2157=EDGE_CURVE('',#1812,#1814,#402,.T.);
#2158=EDGE_CURVE('',#1815,#1814,#403,.T.);
#2159=EDGE_CURVE('',#1813,#1815,#404,.T.);
#2160=EDGE_CURVE('',#1813,#1816,#405,.T.);
#2161=EDGE_CURVE('',#1817,#1815,#406,.T.);
#2162=EDGE_CURVE('',#1816,#1817,#407,.T.);
#2163=EDGE_CURVE('',#1816,#1818,#408,.T.);
#2164=EDGE_CURVE('',#1819,#1817,#409,.T.);
#2165=EDGE_CURVE('',#1818,#1819,#410,.T.);
#2166=EDGE_CURVE('',#1818,#1820,#411,.T.);
#2167=EDGE_CURVE('',#1821,#1819,#412,.T.);
#2168=EDGE_CURVE('',#1820,#1821,#413,.T.);
#2169=EDGE_CURVE('',#1820,#1822,#414,.T.);
#2170=EDGE_CURVE('',#1823,#1821,#415,.T.);
#2171=EDGE_CURVE('',#1822,#1823,#416,.T.);
#2172=EDGE_CURVE('',#1822,#1824,#417,.T.);
#2173=EDGE_CURVE('',#1825,#1823,#418,.T.);
#2174=EDGE_CURVE('',#1824,#1825,#419,.T.);
#2175=EDGE_CURVE('',#1824,#1826,#420,.T.);
#2176=EDGE_CURVE('',#1827,#1825,#421,.T.);
#2177=EDGE_CURVE('',#1826,#1827,#422,.T.);
#2178=EDGE_CURVE('',#1826,#1812,#423,.T.);
#2179=EDGE_CURVE('',#1814,#1827,#424,.T.);
#2180=EDGE_CURVE('',#1828,#1828,#1587,.T.);
#2181=EDGE_CURVE('',#1828,#1829,#425,.T.);
#2182=EDGE_CURVE('',#1829,#1829,#1588,.T.);
#2183=EDGE_CURVE('',#1830,#1830,#1589,.T.);
#2184=EDGE_CURVE('',#1830,#1831,#426,.T.);
#2185=EDGE_CURVE('',#1831,#1831,#1590,.T.);
#2186=EDGE_CURVE('',#1832,#1832,#1591,.T.);
#2187=EDGE_CURVE('',#1832,#1833,#427,.T.);
#2188=EDGE_CURVE('',#1833,#1833,#1592,.T.);
#2189=EDGE_CURVE('',#1834,#1835,#428,.T.);
#2190=EDGE_CURVE('',#1835,#1836,#429,.T.);
#2191=EDGE_CURVE('',#1837,#1836,#430,.T.);
#2192=EDGE_CURVE('',#1834,#1837,#431,.T.);
#2193=EDGE_CURVE('',#1838,#1834,#432,.T.);
#2194=EDGE_CURVE('',#1839,#1837,#433,.T.);
#2195=EDGE_CURVE('',#1838,#1839,#434,.T.);
#2196=EDGE_CURVE('',#1840,#1838,#435,.T.);
#2197=EDGE_CURVE('',#1841,#1839,#436,.T.);
#2198=EDGE_CURVE('',#1840,#1841,#437,.T.);
#2199=EDGE_CURVE('',#1835,#1840,#438,.T.);
#2200=EDGE_CURVE('',#1836,#1841,#439,.T.);
#2201=EDGE_CURVE('',#1842,#1842,#1593,.T.);
#2202=EDGE_CURVE('',#1842,#1843,#440,.T.);
#2203=EDGE_CURVE('',#1843,#1843,#1594,.T.);
#2204=EDGE_CURVE('',#1844,#1844,#1595,.T.);
#2205=EDGE_CURVE('',#1844,#1845,#441,.T.);
#2206=EDGE_CURVE('',#1845,#1845,#1596,.T.);
#2207=EDGE_CURVE('',#1846,#1846,#1597,.T.);
#2208=EDGE_CURVE('',#1846,#1847,#442,.T.);
#2209=EDGE_CURVE('',#1847,#1847,#1598,.T.);
#2210=EDGE_CURVE('',#1848,#1848,#1599,.T.);
#2211=EDGE_CURVE('',#1849,#1849,#1600,.T.);
#2212=EDGE_CURVE('',#1848,#1850,#443,.T.);
#2213=EDGE_CURVE('',#1850,#1850,#1601,.T.);
#2214=EDGE_CURVE('',#1851,#1851,#1602,.T.);
#2215=EDGE_CURVE('',#1851,#1849,#444,.T.);
#2216=EDGE_CURVE('',#1852,#1852,#1603,.T.);
#2217=EDGE_CURVE('',#1852,#1853,#445,.T.);
#2218=EDGE_CURVE('',#1853,#1853,#1604,.T.);
#2219=EDGE_CURVE('',#1854,#1854,#1605,.T.);
#2220=EDGE_CURVE('',#1854,#1855,#446,.T.);
#2221=EDGE_CURVE('',#1855,#1855,#1606,.T.);
#2222=EDGE_CURVE('',#1856,#1856,#1607,.T.);
#2223=EDGE_CURVE('',#1856,#1857,#447,.T.);
#2224=EDGE_CURVE('',#1857,#1857,#1608,.T.);
#2225=EDGE_CURVE('',#1858,#1858,#1609,.T.);
#2226=EDGE_CURVE('',#1858,#1859,#448,.T.);
#2227=EDGE_CURVE('',#1859,#1859,#1610,.T.);
#2228=EDGE_CURVE('',#1860,#1860,#1611,.T.);
#2229=EDGE_CURVE('',#1860,#1861,#449,.T.);
#2230=EDGE_CURVE('',#1861,#1861,#1612,.T.);
#2231=EDGE_CURVE('',#1862,#1862,#1613,.T.);
#2232=EDGE_CURVE('',#1862,#1863,#450,.T.);
#2233=EDGE_CURVE('',#1863,#1863,#1614,.T.);
#2234=EDGE_CURVE('',#1864,#1864,#1615,.T.);
#2235=EDGE_CURVE('',#1864,#1865,#451,.T.);
#2236=EDGE_CURVE('',#1865,#1865,#1616,.T.);
#2237=EDGE_CURVE('',#1866,#1866,#1617,.T.);
#2238=EDGE_CURVE('',#1866,#1867,#452,.T.);
#2239=EDGE_CURVE('',#1867,#1867,#1618,.T.);
#2240=EDGE_CURVE('',#1868,#1869,#453,.T.);
#2241=EDGE_CURVE('',#1869,#1870,#454,.T.);
#2242=EDGE_CURVE('',#1870,#1871,#455,.T.);
#2243=EDGE_CURVE('',#1868,#1871,#456,.T.);
#2244=EDGE_CURVE('',#1869,#1872,#457,.T.);
#2245=EDGE_CURVE('',#1872,#1873,#458,.T.);
#2246=EDGE_CURVE('',#1873,#1870,#459,.T.);
#2247=EDGE_CURVE('',#1872,#1874,#460,.T.);
#2248=EDGE_CURVE('',#1874,#1875,#461,.T.);
#2249=EDGE_CURVE('',#1875,#1873,#462,.T.);
#2250=EDGE_CURVE('',#1874,#1876,#463,.T.);
#2251=EDGE_CURVE('',#1876,#1877,#464,.T.);
#2252=EDGE_CURVE('',#1877,#1875,#465,.T.);
#2253=EDGE_CURVE('',#1876,#1878,#466,.T.);
#2254=EDGE_CURVE('',#1878,#1879,#467,.T.);
#2255=EDGE_CURVE('',#1879,#1877,#468,.T.);
#2256=EDGE_CURVE('',#1878,#1868,#469,.T.);
#2257=EDGE_CURVE('',#1871,#1879,#470,.T.);
#2258=EDGE_CURVE('',#1880,#1880,#1619,.T.);
#2259=EDGE_CURVE('',#1881,#1881,#1620,.T.);
#2260=EDGE_CURVE('',#1880,#1882,#471,.T.);
#2261=EDGE_CURVE('',#1882,#1882,#1621,.T.);
#2262=EDGE_CURVE('',#1883,#1883,#1622,.T.);
#2263=EDGE_CURVE('',#1884,#1884,#1623,.T.);
#2264=EDGE_CURVE('',#1884,#1883,#472,.T.);
#2265=EDGE_CURVE('',#1885,#1885,#1624,.T.);
#2266=EDGE_CURVE('',#1885,#1884,#473,.T.);
#2267=EDGE_CURVE('',#1886,#1886,#1625,.T.);
#2268=EDGE_CURVE('',#1886,#1885,#474,.T.);
#2269=EDGE_CURVE('',#1887,#1887,#1626,.T.);
#2270=EDGE_CURVE('',#1888,#1888,#1627,.F.);
#2271=EDGE_CURVE('',#1888,#1887,#475,.T.);
#2272=EDGE_CURVE('',#1881,#1888,#476,.T.);
#2273=EDGE_CURVE('',#1889,#1889,#1628,.T.);
#2274=EDGE_CURVE('',#1889,#1890,#477,.T.);
#2275=EDGE_CURVE('',#1890,#1890,#1629,.T.);
#2276=EDGE_CURVE('',#1891,#1891,#1630,.T.);
#2277=EDGE_CURVE('',#1891,#1892,#478,.T.);
#2278=EDGE_CURVE('',#1892,#1892,#1631,.T.);
#2279=EDGE_CURVE('',#1893,#1894,#239,.T.);
#2280=EDGE_CURVE('',#1895,#1893,#240,.T.);
#2281=EDGE_CURVE('',#1895,#1896,#479,.T.);
#2282=EDGE_CURVE('',#1896,#1896,#1632,.T.);
#2283=EDGE_CURVE('',#1897,#1895,#241,.T.);
#2284=EDGE_CURVE('',#1898,#1897,#242,.T.);
#2285=EDGE_CURVE('',#1899,#1898,#243,.T.);
#2286=EDGE_CURVE('',#1894,#1899,#244,.T.);
#2287=EDGE_CURVE('',#1900,#1900,#1633,.T.);
#2288=EDGE_CURVE('',#1900,#1901,#480,.T.);
#2289=EDGE_CURVE('',#1902,#1901,#245,.T.);
#2290=EDGE_CURVE('',#1903,#1902,#246,.T.);
#2291=EDGE_CURVE('',#1904,#1903,#247,.T.);
#2292=EDGE_CURVE('',#1905,#1904,#248,.T.);
#2293=EDGE_CURVE('',#1906,#1905,#249,.T.);
#2294=EDGE_CURVE('',#1901,#1906,#250,.T.);
#2295=EDGE_CURVE('',#1897,#1906,#481,.T.);
#2296=EDGE_CURVE('',#1898,#1905,#482,.T.);
#2297=EDGE_CURVE('',#1895,#1901,#483,.T.);
#2298=EDGE_CURVE('',#1893,#1902,#484,.T.);
#2299=EDGE_CURVE('',#1907,#1907,#1634,.F.);
#2300=EDGE_CURVE('',#1907,#1908,#485,.T.);
#2301=EDGE_CURVE('',#1908,#1908,#1635,.F.);
#2302=EDGE_CURVE('',#1894,#1903,#486,.T.);
#2303=EDGE_CURVE('',#1899,#1904,#487,.T.);
#2304=EDGE_CURVE('',#1909,#1909,#1636,.T.);
#2305=EDGE_CURVE('',#1910,#1910,#1637,.T.);
#2306=EDGE_CURVE('',#1910,#1909,#488,.T.);
#2307=EDGE_CURVE('',#1911,#1911,#1638,.T.);
#2308=EDGE_CURVE('',#1911,#1910,#489,.T.);
#2309=EDGE_CURVE('',#1912,#1912,#1639,.T.);
#2310=EDGE_CURVE('',#1912,#1911,#490,.T.);
#2311=EDGE_CURVE('',#1913,#1913,#1640,.T.);
#2312=EDGE_CURVE('',#1914,#1914,#1641,.F.);
#2313=EDGE_CURVE('',#1914,#1913,#491,.T.);
#2314=EDGE_CURVE('',#1915,#1915,#1642,.F.);
#2315=EDGE_CURVE('',#1915,#1914,#492,.T.);
#2316=EDGE_CURVE('',#1916,#1916,#1643,.T.);
#2317=EDGE_CURVE('',#1916,#1915,#493,.T.);
#2318=EDGE_CURVE('',#1917,#1918,#494,.T.);
#2319=EDGE_CURVE('',#1918,#1919,#495,.T.);
#2320=EDGE_CURVE('',#1919,#1920,#496,.T.);
#2321=EDGE_CURVE('',#1917,#1920,#497,.T.);
#2322=EDGE_CURVE('',#1918,#1921,#498,.T.);
#2323=EDGE_CURVE('',#1921,#1922,#499,.T.);
#2324=EDGE_CURVE('',#1922,#1919,#500,.T.);
#2325=EDGE_CURVE('',#1921,#1923,#501,.T.);
#2326=EDGE_CURVE('',#1923,#1924,#502,.T.);
#2327=EDGE_CURVE('',#1924,#1922,#503,.T.);
#2328=EDGE_CURVE('',#1923,#1925,#504,.T.);
#2329=EDGE_CURVE('',#1925,#1926,#505,.T.);
#2330=EDGE_CURVE('',#1926,#1924,#506,.T.);
#2331=EDGE_CURVE('',#1925,#1927,#507,.T.);
#2332=EDGE_CURVE('',#1927,#1928,#508,.T.);
#2333=EDGE_CURVE('',#1928,#1926,#509,.T.);
#2334=EDGE_CURVE('',#1927,#1917,#510,.T.);
#2335=EDGE_CURVE('',#1920,#1928,#511,.T.);
#2336=EDGE_CURVE('',#1929,#1929,#1644,.T.);
#2337=EDGE_CURVE('',#1929,#1930,#512,.T.);
#2338=EDGE_CURVE('',#1930,#1930,#1645,.T.);
#2339=EDGE_CURVE('',#1931,#1931,#1646,.T.);
#2340=EDGE_CURVE('',#1931,#1932,#513,.T.);
#2341=EDGE_CURVE('',#1932,#1932,#1647,.T.);
#2342=EDGE_CURVE('',#1933,#1933,#1648,.T.);
#2343=EDGE_CURVE('',#1933,#1934,#514,.T.);
#2344=EDGE_CURVE('',#1934,#1934,#1649,.T.);
#2345=EDGE_CURVE('',#1935,#1935,#1650,.T.);
#2346=EDGE_CURVE('',#1935,#1936,#515,.T.);
#2347=EDGE_CURVE('',#1936,#1936,#1651,.T.);
#2348=EDGE_CURVE('',#1937,#1937,#1652,.T.);
#2349=EDGE_CURVE('',#1937,#1938,#516,.T.);
#2350=EDGE_CURVE('',#1938,#1938,#1653,.T.);
#2351=EDGE_CURVE('',#1939,#1939,#1654,.T.);
#2352=EDGE_CURVE('',#1939,#1937,#517,.T.);
#2353=EDGE_CURVE('',#1940,#1940,#1655,.T.);
#2354=EDGE_CURVE('',#1940,#1939,#518,.T.);
#2355=EDGE_CURVE('',#1941,#1941,#1656,.T.);
#2356=EDGE_CURVE('',#1942,#1942,#1657,.T.);
#2357=EDGE_CURVE('',#1943,#1943,#1658,.T.);
#2358=EDGE_CURVE('',#1938,#1942,#519,.T.);
#2359=EDGE_CURVE('',#1943,#1944,#520,.T.);
#2360=EDGE_CURVE('',#1944,#1944,#1659,.T.);
#2361=EDGE_CURVE('',#1945,#1945,#1660,.T.);
#2362=EDGE_CURVE('',#1945,#1946,#521,.T.);
#2363=EDGE_CURVE('',#1946,#1946,#1661,.T.);
#2364=EDGE_CURVE('',#1947,#1947,#1662,.T.);
#2365=EDGE_CURVE('',#1947,#1941,#522,.T.);
#2366=EDGE_CURVE('',#1948,#1948,#1663,.T.);
#2367=EDGE_CURVE('',#1948,#1949,#523,.T.);
#2368=EDGE_CURVE('',#1949,#1949,#1664,.T.);
#2369=EDGE_CURVE('',#1950,#1950,#1665,.T.);
#2370=EDGE_CURVE('',#1950,#1951,#524,.T.);
#2371=EDGE_CURVE('',#1951,#1951,#1666,.T.);
#2372=EDGE_CURVE('',#1952,#1953,#1667,.T.);
#2373=EDGE_CURVE('',#1953,#1952,#1668,.T.);
#2374=EDGE_CURVE('',#1953,#1954,#1669,.T.);
#2375=EDGE_CURVE('',#1955,#1954,#1670,.T.);
#2376=EDGE_CURVE('',#1954,#1955,#1671,.T.);
#2377=EDGE_CURVE('',#1955,#1956,#525,.T.);
#2378=EDGE_CURVE('',#1956,#1956,#1672,.T.);
#2379=EDGE_CURVE('',#1957,#1957,#1673,.T.);
#2380=EDGE_CURVE('',#1957,#1958,#526,.T.);
#2381=EDGE_CURVE('',#1958,#1958,#1674,.T.);
#2382=EDGE_CURVE('',#1958,#1959,#527,.T.);
#2383=EDGE_CURVE('',#1959,#1959,#1675,.T.);
#2384=EDGE_CURVE('',#1960,#1960,#1676,.T.);
#2385=EDGE_CURVE('',#1960,#1952,#528,.T.);
#2386=EDGE_CURVE('',#1961,#1961,#1677,.T.);
#2387=EDGE_CURVE('',#1961,#1957,#529,.T.);
#2388=EDGE_CURVE('',#1962,#1963,#1678,.T.);
#2389=EDGE_CURVE('',#1963,#1962,#1679,.T.);
#2390=EDGE_CURVE('',#1963,#1964,#1680,.T.);
#2391=EDGE_CURVE('',#1965,#1964,#1681,.T.);
#2392=EDGE_CURVE('',#1964,#1965,#1682,.T.);
#2393=EDGE_CURVE('',#1966,#1966,#1683,.T.);
#2394=EDGE_CURVE('',#1966,#1965,#530,.T.);
#2395=EDGE_CURVE('',#1967,#1967,#1684,.T.);
#2396=EDGE_CURVE('',#1968,#1968,#1685,.T.);
#2397=EDGE_CURVE('',#1969,#1969,#1686,.T.);
#2398=EDGE_CURVE('',#1969,#1967,#531,.T.);
#2399=EDGE_CURVE('',#1970,#1970,#1687,.T.);
#2400=EDGE_CURVE('',#1970,#1969,#532,.T.);
#2401=EDGE_CURVE('',#1971,#1971,#1688,.T.);
#2402=EDGE_CURVE('',#1971,#1970,#533,.T.);
#2403=EDGE_CURVE('',#1962,#1968,#534,.T.);
#2404=EDGE_CURVE('',#1972,#1973,#1689,.T.);
#2405=EDGE_CURVE('',#1974,#1975,#1690,.T.);
#2406=EDGE_CURVE('',#1976,#1977,#1691,.T.);
#2407=EDGE_CURVE('',#1978,#1979,#1692,.T.);
#2408=EDGE_CURVE('',#1980,#1981,#1693,.T.);
#2409=EDGE_CURVE('',#1982,#1983,#1694,.T.);
#2410=EDGE_CURVE('',#1984,#1985,#1695,.T.);
#2411=EDGE_CURVE('',#1986,#1987,#1696,.T.);
#2412=EDGE_CURVE('',#1988,#1989,#11,.T.);
#2413=EDGE_CURVE('',#1990,#1988,#1697,.T.);
#2414=EDGE_CURVE('',#1991,#1990,#12,.T.);
#2415=EDGE_CURVE('',#1989,#1991,#1698,.T.);
#2416=EDGE_CURVE('',#1992,#1990,#1699,.T.);
#2417=EDGE_CURVE('',#1992,#1993,#13,.T.);
#2418=EDGE_CURVE('',#1994,#1993,#1700,.T.);
#2419=EDGE_CURVE('',#1994,#1995,#14,.T.);
#2420=EDGE_CURVE('',#1996,#1995,#1701,.T.);
#2421=EDGE_CURVE('',#1996,#1997,#15,.T.);
#2422=EDGE_CURVE('',#1997,#1998,#535,.T.);
#2423=EDGE_CURVE('',#1998,#1998,#1702,.T.);
#2424=EDGE_CURVE('',#1997,#1999,#16,.T.);
#2425=EDGE_CURVE('',#2000,#1999,#1703,.T.);
#2426=EDGE_CURVE('',#2000,#2001,#17,.T.);
#2427=EDGE_CURVE('',#2002,#2001,#1704,.T.);
#2428=EDGE_CURVE('',#2002,#2003,#18,.T.);
#2429=EDGE_CURVE('',#2004,#2003,#1705,.T.);
#2430=EDGE_CURVE('',#2004,#2005,#19,.T.);
#2431=EDGE_CURVE('',#2006,#2005,#1706,.T.);
#2432=EDGE_CURVE('',#2006,#2007,#20,.T.);
#2433=EDGE_CURVE('',#1991,#2007,#1707,.T.);
#2434=EDGE_CURVE('',#1988,#2008,#1708,.T.);
#2435=EDGE_CURVE('',#2008,#1992,#1709,.T.);
#2436=EDGE_CURVE('',#2009,#2008,#21,.T.);
#2437=EDGE_CURVE('',#1993,#2009,#1710,.T.);
#2438=EDGE_CURVE('',#2009,#2010,#1711,.T.);
#2439=EDGE_CURVE('',#2010,#1994,#1712,.T.);
#2440=EDGE_CURVE('',#2011,#2010,#22,.T.);
#2441=EDGE_CURVE('',#1995,#2011,#1713,.T.);
#2442=EDGE_CURVE('',#2011,#2012,#1714,.T.);
#2443=EDGE_CURVE('',#2012,#1996,#1715,.T.);
#2444=EDGE_CURVE('',#2013,#2014,#23,.T.);
#2445=EDGE_CURVE('',#1999,#2013,#1716,.T.);
#2446=EDGE_CURVE('',#2014,#2012,#24,.T.);
#2447=EDGE_CURVE('',#2013,#2015,#1717,.T.);
#2448=EDGE_CURVE('',#2015,#2000,#1718,.T.);
#2449=EDGE_CURVE('',#2016,#2015,#25,.T.);
#2450=EDGE_CURVE('',#2001,#2016,#1719,.T.);
#2451=EDGE_CURVE('',#2016,#2017,#1720,.T.);
#2452=EDGE_CURVE('',#2017,#2002,#1721,.T.);
#2453=EDGE_CURVE('',#2018,#2017,#26,.T.);
#2454=EDGE_CURVE('',#2003,#2018,#1722,.T.);
#2455=EDGE_CURVE('',#2018,#2019,#1723,.T.);
#2456=EDGE_CURVE('',#2019,#2004,#1724,.T.);
#2457=EDGE_CURVE('',#2020,#2019,#27,.T.);
#2458=EDGE_CURVE('',#2005,#2020,#1725,.T.);
#2459=EDGE_CURVE('',#2021,#2021,#1726,.T.);
#2460=EDGE_CURVE('',#2021,#2014,#536,.T.);
#2461=EDGE_CURVE('',#2022,#1989,#1727,.T.);
#2462=EDGE_CURVE('',#2022,#2023,#28,.T.);
#2463=EDGE_CURVE('',#2020,#2023,#1728,.T.);
#2464=EDGE_CURVE('',#2007,#2022,#1729,.T.);
#2465=EDGE_CURVE('',#2023,#2006,#1730,.T.);
#2466=EDGE_CURVE('',#2024,#2024,#1731,.T.);
#2467=EDGE_CURVE('',#2025,#2025,#1732,.T.);
#2468=EDGE_CURVE('',#2026,#2026,#1733,.T.);
#2469=EDGE_CURVE('',#2026,#2024,#537,.T.);
#2470=EDGE_CURVE('',#2027,#2027,#1734,.T.);
#2471=EDGE_CURVE('',#2027,#2025,#538,.T.);
#2472=EDGE_CURVE('',#2028,#2028,#1735,.T.);
#2473=EDGE_CURVE('',#2029,#2029,#1736,.T.);
#2474=EDGE_CURVE('',#2030,#2030,#1737,.T.);
#2475=EDGE_CURVE('',#2030,#2028,#539,.T.);
#2476=EDGE_CURVE('',#2031,#2031,#1738,.T.);
#2477=EDGE_CURVE('',#2031,#2029,#540,.T.);
#2478=EDGE_CURVE('',#2032,#2032,#1739,.T.);
#2479=EDGE_CURVE('',#2032,#2033,#541,.T.);
#2480=EDGE_CURVE('',#2033,#2033,#1740,.T.);
#2481=EDGE_CURVE('',#2034,#2034,#1741,.T.);
#2482=EDGE_CURVE('',#2034,#2035,#542,.T.);
#2483=EDGE_CURVE('',#2035,#2035,#1742,.T.);
#2484=EDGE_CURVE('',#2036,#2036,#1743,.T.);
#2485=EDGE_CURVE('',#2036,#2037,#543,.T.);
#2486=EDGE_CURVE('',#2037,#2037,#1744,.T.);
#2487=EDGE_CURVE('',#2038,#2038,#1745,.T.);
#2488=EDGE_CURVE('',#2038,#2039,#544,.T.);
#2489=EDGE_CURVE('',#2039,#2039,#1746,.T.);
#2490=EDGE_CURVE('',#2040,#2040,#1747,.T.);
#2491=EDGE_CURVE('',#2040,#2041,#545,.T.);
#2492=EDGE_CURVE('',#2041,#2041,#1748,.T.);
#2493=EDGE_CURVE('',#2042,#2042,#1749,.T.);
#2494=EDGE_CURVE('',#2042,#2043,#546,.T.);
#2495=EDGE_CURVE('',#2043,#2043,#1750,.T.);
#2496=EDGE_CURVE('',#2044,#2044,#1751,.T.);
#2497=EDGE_CURVE('',#2044,#2045,#547,.T.);
#2498=EDGE_CURVE('',#2045,#2045,#1752,.T.);
#2499=EDGE_CURVE('',#2046,#2047,#548,.T.);
#2500=EDGE_CURVE('',#2047,#2048,#549,.T.);
#2501=EDGE_CURVE('',#2048,#2049,#550,.T.);
#2502=EDGE_CURVE('',#2046,#2049,#551,.T.);
#2503=EDGE_CURVE('',#2047,#2050,#552,.T.);
#2504=EDGE_CURVE('',#2050,#2051,#553,.T.);
#2505=EDGE_CURVE('',#2051,#2048,#554,.T.);
#2506=EDGE_CURVE('',#2050,#2052,#555,.T.);
#2507=EDGE_CURVE('',#2052,#2053,#556,.T.);
#2508=EDGE_CURVE('',#2053,#2051,#557,.T.);
#2509=EDGE_CURVE('',#2052,#2054,#558,.T.);
#2510=EDGE_CURVE('',#2054,#2055,#559,.T.);
#2511=EDGE_CURVE('',#2055,#2053,#560,.T.);
#2512=EDGE_CURVE('',#2054,#2056,#561,.T.);
#2513=EDGE_CURVE('',#2056,#2057,#562,.T.);
#2514=EDGE_CURVE('',#2057,#2055,#563,.T.);
#2515=EDGE_CURVE('',#2056,#2046,#564,.T.);
#2516=EDGE_CURVE('',#2049,#2057,#565,.T.);
#2517=EDGE_CURVE('',#2058,#2058,#1753,.T.);
#2518=EDGE_CURVE('',#2059,#2059,#1754,.T.);
#2519=EDGE_CURVE('',#2060,#2060,#1755,.T.);
#2520=EDGE_CURVE('',#2060,#2059,#566,.T.);
#2521=EDGE_CURVE('',#2061,#2061,#1756,.T.);
#2522=EDGE_CURVE('',#2061,#2060,#567,.T.);
#2523=EDGE_CURVE('',#2062,#2062,#1757,.T.);
#2524=EDGE_CURVE('',#2062,#2061,#568,.T.);
#2525=EDGE_CURVE('',#2063,#2063,#1758,.T.);
#2526=EDGE_CURVE('',#2064,#2064,#1759,.F.);
#2527=EDGE_CURVE('',#2064,#2063,#569,.T.);
#2528=EDGE_CURVE('',#2058,#2064,#570,.T.);
#2529=EDGE_CURVE('',#2065,#2065,#1760,.T.);
#2530=EDGE_CURVE('',#2066,#2066,#1761,.T.);
#2531=EDGE_CURVE('',#2067,#2067,#1762,.T.);
#2532=EDGE_CURVE('',#2068,#2068,#1763,.T.);
#2533=EDGE_CURVE('',#2065,#2067,#571,.T.);
#2534=EDGE_CURVE('',#2068,#2069,#572,.T.);
#2535=EDGE_CURVE('',#2070,#2069,#1764,.T.);
#2536=EDGE_CURVE('',#2071,#2070,#1765,.T.);
#2537=EDGE_CURVE('',#2069,#2071,#1766,.T.);
#2538=EDGE_CURVE('',#2072,#2072,#1767,.T.);
#2539=EDGE_CURVE('',#2072,#2066,#573,.T.);
#2540=EDGE_CURVE('',#2073,#2070,#574,.T.);
#2541=EDGE_CURVE('',#2073,#2074,#575,.T.);
#2542=EDGE_CURVE('',#2071,#2074,#576,.T.);
#2543=EDGE_CURVE('',#2075,#2071,#577,.T.);
#2544=EDGE_CURVE('',#2076,#2075,#578,.T.);
#2545=EDGE_CURVE('',#2070,#2076,#579,.T.);
#2546=EDGE_CURVE('',#2077,#2078,#580,.T.);
#2547=EDGE_CURVE('',#2076,#2077,#581,.T.);
#2548=EDGE_CURVE('',#2078,#2075,#582,.T.);
#2549=EDGE_CURVE('',#2079,#2080,#583,.T.);
#2550=EDGE_CURVE('',#2081,#2079,#584,.T.);
#2551=EDGE_CURVE('',#2082,#2081,#585,.T.);
#2552=EDGE_CURVE('',#2080,#2082,#586,.T.);
#2553=EDGE_CURVE('',#2074,#2081,#587,.T.);
#2554=EDGE_CURVE('',#2079,#2083,#1768,.T.);
#2555=EDGE_CURVE('',#2083,#2084,#588,.T.);
#2556=EDGE_CURVE('',#2084,#2078,#1769,.T.);
#2557=EDGE_CURVE('',#2080,#2085,#1770,.T.);
#2558=EDGE_CURVE('',#2085,#2083,#589,.T.);
#2559=EDGE_CURVE('',#2082,#2073,#590,.T.);
#2560=EDGE_CURVE('',#2086,#2077,#1771,.T.);
#2561=EDGE_CURVE('',#2086,#2085,#591,.T.);
#2562=EDGE_CURVE('',#2084,#2086,#592,.T.);
#2563=EDGE_CURVE('',#2087,#2087,#1772,.T.);
#2564=EDGE_CURVE('',#2087,#2088,#593,.T.);
#2565=EDGE_CURVE('',#2088,#2088,#1773,.T.);
#2566=EDGE_CURVE('',#2089,#2089,#1774,.T.);
#2567=EDGE_CURVE('',#2089,#2090,#594,.T.);
#2568=EDGE_CURVE('',#2090,#2090,#1775,.T.);
#2569=EDGE_CURVE('',#2091,#2091,#1776,.T.);
#2570=EDGE_CURVE('',#2091,#2092,#595,.T.);
#2571=EDGE_CURVE('',#2092,#2092,#1777,.T.);
#2572=EDGE_CURVE('',#2093,#2094,#596,.T.);
#2573=EDGE_CURVE('',#2094,#2095,#597,.T.);
#2574=EDGE_CURVE('',#2096,#2095,#598,.T.);
#2575=EDGE_CURVE('',#2093,#2096,#599,.T.);
#2576=EDGE_CURVE('',#2097,#2093,#600,.T.);
#2577=EDGE_CURVE('',#2098,#2096,#601,.T.);
#2578=EDGE_CURVE('',#2097,#2098,#602,.T.);
#2579=EDGE_CURVE('',#2099,#2097,#603,.T.);
#2580=EDGE_CURVE('',#2100,#2098,#604,.T.);
#2581=EDGE_CURVE('',#2099,#2100,#605,.T.);
#2582=EDGE_CURVE('',#2101,#2099,#606,.T.);
#2583=EDGE_CURVE('',#2102,#2100,#607,.T.);
#2584=EDGE_CURVE('',#2101,#2102,#608,.T.);
#2585=EDGE_CURVE('',#2103,#2101,#609,.T.);
#2586=EDGE_CURVE('',#2104,#2102,#610,.T.);
#2587=EDGE_CURVE('',#2103,#2104,#611,.T.);
#2588=EDGE_CURVE('',#2094,#2103,#612,.T.);
#2589=EDGE_CURVE('',#2095,#2104,#613,.T.);
#2590=ORIENTED_EDGE('',*,*,#2105,.F.);
#2591=ORIENTED_EDGE('',*,*,#2106,.T.);
#2592=ORIENTED_EDGE('',*,*,#2107,.F.);
#2593=ORIENTED_EDGE('',*,*,#2108,.T.);
#2594=ORIENTED_EDGE('',*,*,#2109,.F.);
#2595=ORIENTED_EDGE('',*,*,#2110,.T.);
#2596=ORIENTED_EDGE('',*,*,#2111,.F.);
#2597=ORIENTED_EDGE('',*,*,#2112,.T.);
#2598=ORIENTED_EDGE('',*,*,#2113,.T.);
#2599=ORIENTED_EDGE('',*,*,#2114,.F.);
#2600=ORIENTED_EDGE('',*,*,#2110,.F.);
#2601=ORIENTED_EDGE('',*,*,#2115,.F.);
#2602=ORIENTED_EDGE('',*,*,#2116,.F.);
#2603=ORIENTED_EDGE('',*,*,#2117,.F.);
#2604=ORIENTED_EDGE('',*,*,#2118,.F.);
#2605=ORIENTED_EDGE('',*,*,#2119,.F.);
#2606=ORIENTED_EDGE('',*,*,#2108,.F.);
#2607=ORIENTED_EDGE('',*,*,#2120,.F.);
#2608=ORIENTED_EDGE('',*,*,#2112,.F.);
#2609=ORIENTED_EDGE('',*,*,#2121,.F.);
#2610=ORIENTED_EDGE('',*,*,#2122,.F.);
#2611=ORIENTED_EDGE('',*,*,#2113,.F.);
#2612=ORIENTED_EDGE('',*,*,#2123,.T.);
#2613=ORIENTED_EDGE('',*,*,#2124,.F.);
#2614=ORIENTED_EDGE('',*,*,#2123,.F.);
#2615=ORIENTED_EDGE('',*,*,#2125,.F.);
#2616=ORIENTED_EDGE('',*,*,#2126,.F.);
#2617=ORIENTED_EDGE('',*,*,#2127,.F.);
#2618=ORIENTED_EDGE('',*,*,#2106,.F.);
#2619=ORIENTED_EDGE('',*,*,#2128,.F.);
#2620=ORIENTED_EDGE('',*,*,#2129,.T.);
#2621=ORIENTED_EDGE('',*,*,#2130,.F.);
#2622=ORIENTED_EDGE('',*,*,#2125,.T.);
#2623=ORIENTED_EDGE('',*,*,#2105,.T.);
#2624=ORIENTED_EDGE('',*,*,#2120,.T.);
#2625=ORIENTED_EDGE('',*,*,#2131,.F.);
#2626=ORIENTED_EDGE('',*,*,#2129,.F.);
#2627=ORIENTED_EDGE('',*,*,#2132,.F.);
#2628=ORIENTED_EDGE('',*,*,#2133,.T.);
#2629=ORIENTED_EDGE('',*,*,#2134,.F.);
#2630=ORIENTED_EDGE('',*,*,#2121,.T.);
#2631=ORIENTED_EDGE('',*,*,#2111,.T.);
#2632=ORIENTED_EDGE('',*,*,#2114,.T.);
#2633=ORIENTED_EDGE('',*,*,#2135,.F.);
#2634=ORIENTED_EDGE('',*,*,#2133,.F.);
#2635=ORIENTED_EDGE('',*,*,#2136,.F.);
#2636=ORIENTED_EDGE('',*,*,#2137,.T.);
#2637=ORIENTED_EDGE('',*,*,#2138,.F.);
#2638=ORIENTED_EDGE('',*,*,#2115,.T.);
#2639=ORIENTED_EDGE('',*,*,#2109,.T.);
#2640=ORIENTED_EDGE('',*,*,#2119,.T.);
#2641=ORIENTED_EDGE('',*,*,#2139,.F.);
#2642=ORIENTED_EDGE('',*,*,#2137,.F.);
#2643=ORIENTED_EDGE('',*,*,#2124,.T.);
#2644=ORIENTED_EDGE('',*,*,#2140,.T.);
#2645=ORIENTED_EDGE('',*,*,#2141,.F.);
#2646=ORIENTED_EDGE('',*,*,#2142,.T.);
#2647=ORIENTED_EDGE('',*,*,#2143,.F.);
#2648=ORIENTED_EDGE('',*,*,#2117,.T.);
#2649=ORIENTED_EDGE('',*,*,#2107,.T.);
#2650=ORIENTED_EDGE('',*,*,#2127,.T.);
#2651=ORIENTED_EDGE('',*,*,#2144,.F.);
#2652=ORIENTED_EDGE('',*,*,#2142,.F.);
#2653=ORIENTED_EDGE('',*,*,#2145,.F.);
#2654=ORIENTED_EDGE('',*,*,#2146,.T.);
#2655=ORIENTED_EDGE('',*,*,#2147,.F.);
#2656=ORIENTED_EDGE('',*,*,#2146,.F.);
#2657=ORIENTED_EDGE('',*,*,#2148,.F.);
#2658=ORIENTED_EDGE('',*,*,#2149,.T.);
#2659=ORIENTED_EDGE('',*,*,#2150,.F.);
#2660=ORIENTED_EDGE('',*,*,#2149,.F.);
#2661=ORIENTED_EDGE('',*,*,#2151,.F.);
#2662=ORIENTED_EDGE('',*,*,#2152,.T.);
#2663=ORIENTED_EDGE('',*,*,#2153,.F.);
#2664=ORIENTED_EDGE('',*,*,#2152,.F.);
#2665=ORIENTED_EDGE('',*,*,#2154,.F.);
#2666=ORIENTED_EDGE('',*,*,#2155,.T.);
#2667=ORIENTED_EDGE('',*,*,#2140,.F.);
#2668=ORIENTED_EDGE('',*,*,#2155,.F.);
#2669=ORIENTED_EDGE('',*,*,#2156,.F.);
#2670=ORIENTED_EDGE('',*,*,#2157,.T.);
#2671=ORIENTED_EDGE('',*,*,#2158,.F.);
#2672=ORIENTED_EDGE('',*,*,#2159,.F.);
#2673=ORIENTED_EDGE('',*,*,#2160,.F.);
#2674=ORIENTED_EDGE('',*,*,#2159,.T.);
#2675=ORIENTED_EDGE('',*,*,#2161,.F.);
#2676=ORIENTED_EDGE('',*,*,#2162,.F.);
#2677=ORIENTED_EDGE('',*,*,#2163,.F.);
#2678=ORIENTED_EDGE('',*,*,#2162,.T.);
#2679=ORIENTED_EDGE('',*,*,#2164,.F.);
#2680=ORIENTED_EDGE('',*,*,#2165,.F.);
#2681=ORIENTED_EDGE('',*,*,#2166,.F.);
#2682=ORIENTED_EDGE('',*,*,#2165,.T.);
#2683=ORIENTED_EDGE('',*,*,#2167,.F.);
#2684=ORIENTED_EDGE('',*,*,#2168,.F.);
#2685=ORIENTED_EDGE('',*,*,#2169,.F.);
#2686=ORIENTED_EDGE('',*,*,#2168,.T.);
#2687=ORIENTED_EDGE('',*,*,#2170,.F.);
#2688=ORIENTED_EDGE('',*,*,#2171,.F.);
#2689=ORIENTED_EDGE('',*,*,#2172,.F.);
#2690=ORIENTED_EDGE('',*,*,#2171,.T.);
#2691=ORIENTED_EDGE('',*,*,#2173,.F.);
#2692=ORIENTED_EDGE('',*,*,#2174,.F.);
#2693=ORIENTED_EDGE('',*,*,#2175,.F.);
#2694=ORIENTED_EDGE('',*,*,#2174,.T.);
#2695=ORIENTED_EDGE('',*,*,#2176,.F.);
#2696=ORIENTED_EDGE('',*,*,#2177,.F.);
#2697=ORIENTED_EDGE('',*,*,#2178,.F.);
#2698=ORIENTED_EDGE('',*,*,#2177,.T.);
#2699=ORIENTED_EDGE('',*,*,#2179,.F.);
#2700=ORIENTED_EDGE('',*,*,#2157,.F.);
#2701=ORIENTED_EDGE('',*,*,#2179,.T.);
#2702=ORIENTED_EDGE('',*,*,#2176,.T.);
#2703=ORIENTED_EDGE('',*,*,#2173,.T.);
#2704=ORIENTED_EDGE('',*,*,#2170,.T.);
#2705=ORIENTED_EDGE('',*,*,#2167,.T.);
#2706=ORIENTED_EDGE('',*,*,#2164,.T.);
#2707=ORIENTED_EDGE('',*,*,#2161,.T.);
#2708=ORIENTED_EDGE('',*,*,#2158,.T.);
#2709=ORIENTED_EDGE('',*,*,#2126,.T.);
#2710=ORIENTED_EDGE('',*,*,#2130,.T.);
#2711=ORIENTED_EDGE('',*,*,#2131,.T.);
#2712=ORIENTED_EDGE('',*,*,#2122,.T.);
#2713=ORIENTED_EDGE('',*,*,#2134,.T.);
#2714=ORIENTED_EDGE('',*,*,#2135,.T.);
#2715=ORIENTED_EDGE('',*,*,#2116,.T.);
#2716=ORIENTED_EDGE('',*,*,#2138,.T.);
#2717=ORIENTED_EDGE('',*,*,#2139,.T.);
#2718=ORIENTED_EDGE('',*,*,#2118,.T.);
#2719=ORIENTED_EDGE('',*,*,#2143,.T.);
#2720=ORIENTED_EDGE('',*,*,#2144,.T.);
#2721=ORIENTED_EDGE('',*,*,#2153,.T.);
#2722=ORIENTED_EDGE('',*,*,#2150,.T.);
#2723=ORIENTED_EDGE('',*,*,#2147,.T.);
#2724=ORIENTED_EDGE('',*,*,#2178,.T.);
#2725=ORIENTED_EDGE('',*,*,#2156,.T.);
#2726=ORIENTED_EDGE('',*,*,#2160,.T.);
#2727=ORIENTED_EDGE('',*,*,#2163,.T.);
#2728=ORIENTED_EDGE('',*,*,#2166,.T.);
#2729=ORIENTED_EDGE('',*,*,#2169,.T.);
#2730=ORIENTED_EDGE('',*,*,#2172,.T.);
#2731=ORIENTED_EDGE('',*,*,#2175,.T.);
#2732=ORIENTED_EDGE('',*,*,#2154,.T.);
#2733=ORIENTED_EDGE('',*,*,#2151,.T.);
#2734=ORIENTED_EDGE('',*,*,#2148,.T.);
#2735=ORIENTED_EDGE('',*,*,#2145,.T.);
#2736=ORIENTED_EDGE('',*,*,#2136,.T.);
#2737=ORIENTED_EDGE('',*,*,#2128,.T.);
#2738=ORIENTED_EDGE('',*,*,#2141,.T.);
#2739=ORIENTED_EDGE('',*,*,#2132,.T.);
#2740=ORIENTED_EDGE('',*,*,#2180,.F.);
#2741=ORIENTED_EDGE('',*,*,#2181,.T.);
#2742=ORIENTED_EDGE('',*,*,#2182,.F.);
#2743=ORIENTED_EDGE('',*,*,#2181,.F.);
#2744=ORIENTED_EDGE('',*,*,#2183,.F.);
#2745=ORIENTED_EDGE('',*,*,#2184,.T.);
#2746=ORIENTED_EDGE('',*,*,#2185,.F.);
#2747=ORIENTED_EDGE('',*,*,#2184,.F.);
#2748=ORIENTED_EDGE('',*,*,#2186,.F.);
#2749=ORIENTED_EDGE('',*,*,#2187,.T.);
#2750=ORIENTED_EDGE('',*,*,#2188,.F.);
#2751=ORIENTED_EDGE('',*,*,#2187,.F.);
#2752=ORIENTED_EDGE('',*,*,#2189,.T.);
#2753=ORIENTED_EDGE('',*,*,#2190,.T.);
#2754=ORIENTED_EDGE('',*,*,#2191,.F.);
#2755=ORIENTED_EDGE('',*,*,#2192,.F.);
#2756=ORIENTED_EDGE('',*,*,#2185,.T.);
#2757=ORIENTED_EDGE('',*,*,#2188,.T.);
#2758=ORIENTED_EDGE('',*,*,#2193,.T.);
#2759=ORIENTED_EDGE('',*,*,#2192,.T.);
#2760=ORIENTED_EDGE('',*,*,#2194,.F.);
#2761=ORIENTED_EDGE('',*,*,#2195,.F.);
#2762=ORIENTED_EDGE('',*,*,#2196,.T.);
#2763=ORIENTED_EDGE('',*,*,#2195,.T.);
#2764=ORIENTED_EDGE('',*,*,#2197,.F.);
#2765=ORIENTED_EDGE('',*,*,#2198,.F.);
#2766=ORIENTED_EDGE('',*,*,#2183,.T.);
#2767=ORIENTED_EDGE('',*,*,#2186,.T.);
#2768=ORIENTED_EDGE('',*,*,#2199,.T.);
#2769=ORIENTED_EDGE('',*,*,#2198,.T.);
#2770=ORIENTED_EDGE('',*,*,#2200,.F.);
#2771=ORIENTED_EDGE('',*,*,#2190,.F.);
#2772=ORIENTED_EDGE('',*,*,#2200,.T.);
#2773=ORIENTED_EDGE('',*,*,#2197,.T.);
#2774=ORIENTED_EDGE('',*,*,#2194,.T.);
#2775=ORIENTED_EDGE('',*,*,#2191,.T.);
#2776=ORIENTED_EDGE('',*,*,#2182,.T.);
#2777=ORIENTED_EDGE('',*,*,#2199,.F.);
#2778=ORIENTED_EDGE('',*,*,#2189,.F.);
#2779=ORIENTED_EDGE('',*,*,#2193,.F.);
#2780=ORIENTED_EDGE('',*,*,#2196,.F.);
#2781=ORIENTED_EDGE('',*,*,#2180,.T.);
#2782=ORIENTED_EDGE('',*,*,#2201,.F.);
#2783=ORIENTED_EDGE('',*,*,#2202,.T.);
#2784=ORIENTED_EDGE('',*,*,#2203,.T.);
#2785=ORIENTED_EDGE('',*,*,#2202,.F.);
#2786=ORIENTED_EDGE('',*,*,#2204,.F.);
#2787=ORIENTED_EDGE('',*,*,#2205,.T.);
#2788=ORIENTED_EDGE('',*,*,#2206,.T.);
#2789=ORIENTED_EDGE('',*,*,#2205,.F.);
#2790=ORIENTED_EDGE('',*,*,#2204,.T.);
#2791=ORIENTED_EDGE('',*,*,#2201,.T.);
#2792=ORIENTED_EDGE('',*,*,#2206,.F.);
#2793=ORIENTED_EDGE('',*,*,#2203,.F.);
#2794=ORIENTED_EDGE('',*,*,#2207,.F.);
#2795=ORIENTED_EDGE('',*,*,#2208,.T.);
#2796=ORIENTED_EDGE('',*,*,#2209,.F.);
#2797=ORIENTED_EDGE('',*,*,#2208,.F.);
#2798=ORIENTED_EDGE('',*,*,#2207,.T.);
#2799=ORIENTED_EDGE('',*,*,#2210,.T.);
#2800=ORIENTED_EDGE('',*,*,#2211,.F.);
#2801=ORIENTED_EDGE('',*,*,#2210,.F.);
#2802=ORIENTED_EDGE('',*,*,#2212,.T.);
#2803=ORIENTED_EDGE('',*,*,#2213,.T.);
#2804=ORIENTED_EDGE('',*,*,#2212,.F.);
#2805=ORIENTED_EDGE('',*,*,#2213,.F.);
#2806=ORIENTED_EDGE('',*,*,#2214,.F.);
#2807=ORIENTED_EDGE('',*,*,#2215,.T.);
#2808=ORIENTED_EDGE('',*,*,#2211,.T.);
#2809=ORIENTED_EDGE('',*,*,#2215,.F.);
#2810=ORIENTED_EDGE('',*,*,#2214,.T.);
#2811=ORIENTED_EDGE('',*,*,#2209,.T.);
#2812=ORIENTED_EDGE('',*,*,#2216,.F.);
#2813=ORIENTED_EDGE('',*,*,#2217,.T.);
#2814=ORIENTED_EDGE('',*,*,#2218,.T.);
#2815=ORIENTED_EDGE('',*,*,#2217,.F.);
#2816=ORIENTED_EDGE('',*,*,#2219,.F.);
#2817=ORIENTED_EDGE('',*,*,#2220,.T.);
#2818=ORIENTED_EDGE('',*,*,#2221,.T.);
#2819=ORIENTED_EDGE('',*,*,#2220,.F.);
#2820=ORIENTED_EDGE('',*,*,#2219,.T.);
#2821=ORIENTED_EDGE('',*,*,#2216,.T.);
#2822=ORIENTED_EDGE('',*,*,#2221,.F.);
#2823=ORIENTED_EDGE('',*,*,#2218,.F.);
#2824=ORIENTED_EDGE('',*,*,#2222,.F.);
#2825=ORIENTED_EDGE('',*,*,#2223,.T.);
#2826=ORIENTED_EDGE('',*,*,#2224,.T.);
#2827=ORIENTED_EDGE('',*,*,#2223,.F.);
#2828=ORIENTED_EDGE('',*,*,#2225,.F.);
#2829=ORIENTED_EDGE('',*,*,#2226,.T.);
#2830=ORIENTED_EDGE('',*,*,#2227,.T.);
#2831=ORIENTED_EDGE('',*,*,#2226,.F.);
#2832=ORIENTED_EDGE('',*,*,#2225,.T.);
#2833=ORIENTED_EDGE('',*,*,#2222,.T.);
#2834=ORIENTED_EDGE('',*,*,#2227,.F.);
#2835=ORIENTED_EDGE('',*,*,#2224,.F.);
#2836=ORIENTED_EDGE('',*,*,#2228,.F.);
#2837=ORIENTED_EDGE('',*,*,#2229,.T.);
#2838=ORIENTED_EDGE('',*,*,#2230,.T.);
#2839=ORIENTED_EDGE('',*,*,#2229,.F.);
#2840=ORIENTED_EDGE('',*,*,#2231,.F.);
#2841=ORIENTED_EDGE('',*,*,#2232,.T.);
#2842=ORIENTED_EDGE('',*,*,#2233,.T.);
#2843=ORIENTED_EDGE('',*,*,#2232,.F.);
#2844=ORIENTED_EDGE('',*,*,#2231,.T.);
#2845=ORIENTED_EDGE('',*,*,#2228,.T.);
#2846=ORIENTED_EDGE('',*,*,#2233,.F.);
#2847=ORIENTED_EDGE('',*,*,#2230,.F.);
#2848=ORIENTED_EDGE('',*,*,#2234,.F.);
#2849=ORIENTED_EDGE('',*,*,#2235,.T.);
#2850=ORIENTED_EDGE('',*,*,#2236,.T.);
#2851=ORIENTED_EDGE('',*,*,#2235,.F.);
#2852=ORIENTED_EDGE('',*,*,#2237,.F.);
#2853=ORIENTED_EDGE('',*,*,#2238,.T.);
#2854=ORIENTED_EDGE('',*,*,#2239,.T.);
#2855=ORIENTED_EDGE('',*,*,#2238,.F.);
#2856=ORIENTED_EDGE('',*,*,#2237,.T.);
#2857=ORIENTED_EDGE('',*,*,#2234,.T.);
#2858=ORIENTED_EDGE('',*,*,#2239,.F.);
#2859=ORIENTED_EDGE('',*,*,#2236,.F.);
#2860=ORIENTED_EDGE('',*,*,#2240,.T.);
#2861=ORIENTED_EDGE('',*,*,#2241,.T.);
#2862=ORIENTED_EDGE('',*,*,#2242,.T.);
#2863=ORIENTED_EDGE('',*,*,#2243,.F.);
#2864=ORIENTED_EDGE('',*,*,#2244,.T.);
#2865=ORIENTED_EDGE('',*,*,#2245,.T.);
#2866=ORIENTED_EDGE('',*,*,#2246,.T.);
#2867=ORIENTED_EDGE('',*,*,#2241,.F.);
#2868=ORIENTED_EDGE('',*,*,#2247,.T.);
#2869=ORIENTED_EDGE('',*,*,#2248,.T.);
#2870=ORIENTED_EDGE('',*,*,#2249,.T.);
#2871=ORIENTED_EDGE('',*,*,#2245,.F.);
#2872=ORIENTED_EDGE('',*,*,#2250,.T.);
#2873=ORIENTED_EDGE('',*,*,#2251,.T.);
#2874=ORIENTED_EDGE('',*,*,#2252,.T.);
#2875=ORIENTED_EDGE('',*,*,#2248,.F.);
#2876=ORIENTED_EDGE('',*,*,#2253,.T.);
#2877=ORIENTED_EDGE('',*,*,#2254,.T.);
#2878=ORIENTED_EDGE('',*,*,#2255,.T.);
#2879=ORIENTED_EDGE('',*,*,#2251,.F.);
#2880=ORIENTED_EDGE('',*,*,#2256,.T.);
#2881=ORIENTED_EDGE('',*,*,#2243,.T.);
#2882=ORIENTED_EDGE('',*,*,#2257,.T.);
#2883=ORIENTED_EDGE('',*,*,#2254,.F.);
#2884=ORIENTED_EDGE('',*,*,#2256,.F.);
#2885=ORIENTED_EDGE('',*,*,#2253,.F.);
#2886=ORIENTED_EDGE('',*,*,#2250,.F.);
#2887=ORIENTED_EDGE('',*,*,#2247,.F.);
#2888=ORIENTED_EDGE('',*,*,#2244,.F.);
#2889=ORIENTED_EDGE('',*,*,#2240,.F.);
#2890=ORIENTED_EDGE('',*,*,#2257,.F.);
#2891=ORIENTED_EDGE('',*,*,#2242,.F.);
#2892=ORIENTED_EDGE('',*,*,#2246,.F.);
#2893=ORIENTED_EDGE('',*,*,#2249,.F.);
#2894=ORIENTED_EDGE('',*,*,#2252,.F.);
#2895=ORIENTED_EDGE('',*,*,#2255,.F.);
#2896=ORIENTED_EDGE('',*,*,#2258,.T.);
#2897=ORIENTED_EDGE('',*,*,#2259,.F.);
#2898=ORIENTED_EDGE('',*,*,#2258,.F.);
#2899=ORIENTED_EDGE('',*,*,#2260,.T.);
#2900=ORIENTED_EDGE('',*,*,#2261,.T.);
#2901=ORIENTED_EDGE('',*,*,#2260,.F.);
#2902=ORIENTED_EDGE('',*,*,#2261,.F.);
#2903=ORIENTED_EDGE('',*,*,#2262,.F.);
#2904=ORIENTED_EDGE('',*,*,#2263,.F.);
#2905=ORIENTED_EDGE('',*,*,#2264,.T.);
#2906=ORIENTED_EDGE('',*,*,#2262,.T.);
#2907=ORIENTED_EDGE('',*,*,#2264,.F.);
#2908=ORIENTED_EDGE('',*,*,#2265,.F.);
#2909=ORIENTED_EDGE('',*,*,#2266,.T.);
#2910=ORIENTED_EDGE('',*,*,#2263,.T.);
#2911=ORIENTED_EDGE('',*,*,#2266,.F.);
#2912=ORIENTED_EDGE('',*,*,#2267,.F.);
#2913=ORIENTED_EDGE('',*,*,#2268,.T.);
#2914=ORIENTED_EDGE('',*,*,#2265,.T.);
#2915=ORIENTED_EDGE('',*,*,#2268,.F.);
#2916=ORIENTED_EDGE('',*,*,#2267,.T.);
#2917=ORIENTED_EDGE('',*,*,#2269,.F.);
#2918=ORIENTED_EDGE('',*,*,#2270,.F.);
#2919=ORIENTED_EDGE('',*,*,#2271,.T.);
#2920=ORIENTED_EDGE('',*,*,#2269,.T.);
#2921=ORIENTED_EDGE('',*,*,#2271,.F.);
#2922=ORIENTED_EDGE('',*,*,#2259,.T.);
#2923=ORIENTED_EDGE('',*,*,#2272,.T.);
#2924=ORIENTED_EDGE('',*,*,#2270,.T.);
#2925=ORIENTED_EDGE('',*,*,#2272,.F.);
#2926=ORIENTED_EDGE('',*,*,#2273,.F.);
#2927=ORIENTED_EDGE('',*,*,#2274,.T.);
#2928=ORIENTED_EDGE('',*,*,#2275,.T.);
#2929=ORIENTED_EDGE('',*,*,#2274,.F.);
#2930=ORIENTED_EDGE('',*,*,#2276,.F.);
#2931=ORIENTED_EDGE('',*,*,#2277,.T.);
#2932=ORIENTED_EDGE('',*,*,#2278,.T.);
#2933=ORIENTED_EDGE('',*,*,#2277,.F.);
#2934=ORIENTED_EDGE('',*,*,#2276,.T.);
#2935=ORIENTED_EDGE('',*,*,#2273,.T.);
#2936=ORIENTED_EDGE('',*,*,#2278,.F.);
#2937=ORIENTED_EDGE('',*,*,#2275,.F.);
#2938=ORIENTED_EDGE('',*,*,#2279,.F.);
#2939=ORIENTED_EDGE('',*,*,#2280,.F.);
#2940=ORIENTED_EDGE('',*,*,#2281,.T.);
#2941=ORIENTED_EDGE('',*,*,#2282,.F.);
#2942=ORIENTED_EDGE('',*,*,#2281,.F.);
#2943=ORIENTED_EDGE('',*,*,#2283,.F.);
#2944=ORIENTED_EDGE('',*,*,#2284,.F.);
#2945=ORIENTED_EDGE('',*,*,#2285,.F.);
#2946=ORIENTED_EDGE('',*,*,#2286,.F.);
#2947=ORIENTED_EDGE('',*,*,#2287,.F.);
#2948=ORIENTED_EDGE('',*,*,#2288,.T.);
#2949=ORIENTED_EDGE('',*,*,#2289,.F.);
#2950=ORIENTED_EDGE('',*,*,#2290,.F.);
#2951=ORIENTED_EDGE('',*,*,#2291,.F.);
#2952=ORIENTED_EDGE('',*,*,#2292,.F.);
#2953=ORIENTED_EDGE('',*,*,#2293,.F.);
#2954=ORIENTED_EDGE('',*,*,#2294,.F.);
#2955=ORIENTED_EDGE('',*,*,#2288,.F.);
#2956=ORIENTED_EDGE('',*,*,#2284,.T.);
#2957=ORIENTED_EDGE('',*,*,#2295,.T.);
#2958=ORIENTED_EDGE('',*,*,#2293,.T.);
#2959=ORIENTED_EDGE('',*,*,#2296,.F.);
#2960=ORIENTED_EDGE('',*,*,#2283,.T.);
#2961=ORIENTED_EDGE('',*,*,#2297,.T.);
#2962=ORIENTED_EDGE('',*,*,#2294,.T.);
#2963=ORIENTED_EDGE('',*,*,#2295,.F.);
#2964=ORIENTED_EDGE('',*,*,#2280,.T.);
#2965=ORIENTED_EDGE('',*,*,#2298,.T.);
#2966=ORIENTED_EDGE('',*,*,#2289,.T.);
#2967=ORIENTED_EDGE('',*,*,#2297,.F.);
#2968=ORIENTED_EDGE('',*,*,#2299,.F.);
#2969=ORIENTED_EDGE('',*,*,#2300,.T.);
#2970=ORIENTED_EDGE('',*,*,#2301,.T.);
#2971=ORIENTED_EDGE('',*,*,#2300,.F.);
#2972=ORIENTED_EDGE('',*,*,#2279,.T.);
#2973=ORIENTED_EDGE('',*,*,#2302,.T.);
#2974=ORIENTED_EDGE('',*,*,#2290,.T.);
#2975=ORIENTED_EDGE('',*,*,#2298,.F.);
#2976=ORIENTED_EDGE('',*,*,#2285,.T.);
#2977=ORIENTED_EDGE('',*,*,#2296,.T.);
#2978=ORIENTED_EDGE('',*,*,#2292,.T.);
#2979=ORIENTED_EDGE('',*,*,#2303,.F.);
#2980=ORIENTED_EDGE('',*,*,#2286,.T.);
#2981=ORIENTED_EDGE('',*,*,#2303,.T.);
#2982=ORIENTED_EDGE('',*,*,#2291,.T.);
#2983=ORIENTED_EDGE('',*,*,#2302,.F.);
#2984=ORIENTED_EDGE('',*,*,#2287,.T.);
#2985=ORIENTED_EDGE('',*,*,#2299,.T.);
#2986=ORIENTED_EDGE('',*,*,#2282,.T.);
#2987=ORIENTED_EDGE('',*,*,#2301,.F.);
#2988=ORIENTED_EDGE('',*,*,#2304,.F.);
#2989=ORIENTED_EDGE('',*,*,#2305,.F.);
#2990=ORIENTED_EDGE('',*,*,#2306,.T.);
#2991=ORIENTED_EDGE('',*,*,#2304,.T.);
#2992=ORIENTED_EDGE('',*,*,#2306,.F.);
#2993=ORIENTED_EDGE('',*,*,#2307,.F.);
#2994=ORIENTED_EDGE('',*,*,#2308,.T.);
#2995=ORIENTED_EDGE('',*,*,#2305,.T.);
#2996=ORIENTED_EDGE('',*,*,#2308,.F.);
#2997=ORIENTED_EDGE('',*,*,#2309,.F.);
#2998=ORIENTED_EDGE('',*,*,#2310,.T.);
#2999=ORIENTED_EDGE('',*,*,#2307,.T.);
#3000=ORIENTED_EDGE('',*,*,#2310,.F.);
#3001=ORIENTED_EDGE('',*,*,#2309,.T.);
#3002=ORIENTED_EDGE('',*,*,#2311,.F.);
#3003=ORIENTED_EDGE('',*,*,#2312,.F.);
#3004=ORIENTED_EDGE('',*,*,#2313,.T.);
#3005=ORIENTED_EDGE('',*,*,#2311,.T.);
#3006=ORIENTED_EDGE('',*,*,#2313,.F.);
#3007=ORIENTED_EDGE('',*,*,#2314,.F.);
#3008=ORIENTED_EDGE('',*,*,#2315,.T.);
#3009=ORIENTED_EDGE('',*,*,#2312,.T.);
#3010=ORIENTED_EDGE('',*,*,#2315,.F.);
#3011=ORIENTED_EDGE('',*,*,#2316,.F.);
#3012=ORIENTED_EDGE('',*,*,#2317,.T.);
#3013=ORIENTED_EDGE('',*,*,#2314,.T.);
#3014=ORIENTED_EDGE('',*,*,#2317,.F.);
#3015=ORIENTED_EDGE('',*,*,#2316,.T.);
#3016=ORIENTED_EDGE('',*,*,#2318,.T.);
#3017=ORIENTED_EDGE('',*,*,#2319,.T.);
#3018=ORIENTED_EDGE('',*,*,#2320,.T.);
#3019=ORIENTED_EDGE('',*,*,#2321,.F.);
#3020=ORIENTED_EDGE('',*,*,#2322,.T.);
#3021=ORIENTED_EDGE('',*,*,#2323,.T.);
#3022=ORIENTED_EDGE('',*,*,#2324,.T.);
#3023=ORIENTED_EDGE('',*,*,#2319,.F.);
#3024=ORIENTED_EDGE('',*,*,#2325,.T.);
#3025=ORIENTED_EDGE('',*,*,#2326,.T.);
#3026=ORIENTED_EDGE('',*,*,#2327,.T.);
#3027=ORIENTED_EDGE('',*,*,#2323,.F.);
#3028=ORIENTED_EDGE('',*,*,#2328,.T.);
#3029=ORIENTED_EDGE('',*,*,#2329,.T.);
#3030=ORIENTED_EDGE('',*,*,#2330,.T.);
#3031=ORIENTED_EDGE('',*,*,#2326,.F.);
#3032=ORIENTED_EDGE('',*,*,#2331,.T.);
#3033=ORIENTED_EDGE('',*,*,#2332,.T.);
#3034=ORIENTED_EDGE('',*,*,#2333,.T.);
#3035=ORIENTED_EDGE('',*,*,#2329,.F.);
#3036=ORIENTED_EDGE('',*,*,#2334,.T.);
#3037=ORIENTED_EDGE('',*,*,#2321,.T.);
#3038=ORIENTED_EDGE('',*,*,#2335,.T.);
#3039=ORIENTED_EDGE('',*,*,#2332,.F.);
#3040=ORIENTED_EDGE('',*,*,#2334,.F.);
#3041=ORIENTED_EDGE('',*,*,#2331,.F.);
#3042=ORIENTED_EDGE('',*,*,#2328,.F.);
#3043=ORIENTED_EDGE('',*,*,#2325,.F.);
#3044=ORIENTED_EDGE('',*,*,#2322,.F.);
#3045=ORIENTED_EDGE('',*,*,#2318,.F.);
#3046=ORIENTED_EDGE('',*,*,#2335,.F.);
#3047=ORIENTED_EDGE('',*,*,#2320,.F.);
#3048=ORIENTED_EDGE('',*,*,#2324,.F.);
#3049=ORIENTED_EDGE('',*,*,#2327,.F.);
#3050=ORIENTED_EDGE('',*,*,#2330,.F.);
#3051=ORIENTED_EDGE('',*,*,#2333,.F.);
#3052=ORIENTED_EDGE('',*,*,#2336,.F.);
#3053=ORIENTED_EDGE('',*,*,#2337,.T.);
#3054=ORIENTED_EDGE('',*,*,#2338,.F.);
#3055=ORIENTED_EDGE('',*,*,#2337,.F.);
#3056=ORIENTED_EDGE('',*,*,#2339,.F.);
#3057=ORIENTED_EDGE('',*,*,#2340,.T.);
#3058=ORIENTED_EDGE('',*,*,#2341,.F.);
#3059=ORIENTED_EDGE('',*,*,#2340,.F.);
#3060=ORIENTED_EDGE('',*,*,#2342,.F.);
#3061=ORIENTED_EDGE('',*,*,#2343,.T.);
#3062=ORIENTED_EDGE('',*,*,#2344,.F.);
#3063=ORIENTED_EDGE('',*,*,#2343,.F.);
#3064=ORIENTED_EDGE('',*,*,#2345,.F.);
#3065=ORIENTED_EDGE('',*,*,#2346,.T.);
#3066=ORIENTED_EDGE('',*,*,#2347,.F.);
#3067=ORIENTED_EDGE('',*,*,#2346,.F.);
#3068=ORIENTED_EDGE('',*,*,#2348,.T.);
#3069=ORIENTED_EDGE('',*,*,#2349,.T.);
#3070=ORIENTED_EDGE('',*,*,#2350,.F.);
#3071=ORIENTED_EDGE('',*,*,#2349,.F.);
#3072=ORIENTED_EDGE('',*,*,#2351,.F.);
#3073=ORIENTED_EDGE('',*,*,#2352,.T.);
#3074=ORIENTED_EDGE('',*,*,#2348,.F.);
#3075=ORIENTED_EDGE('',*,*,#2352,.F.);
#3076=ORIENTED_EDGE('',*,*,#2353,.F.);
#3077=ORIENTED_EDGE('',*,*,#2354,.T.);
#3078=ORIENTED_EDGE('',*,*,#2351,.T.);
#3079=ORIENTED_EDGE('',*,*,#2354,.F.);
#3080=ORIENTED_EDGE('',*,*,#2353,.T.);
#3081=ORIENTED_EDGE('',*,*,#2355,.F.);
#3082=ORIENTED_EDGE('',*,*,#2356,.F.);
#3083=ORIENTED_EDGE('',*,*,#2357,.F.);
#3084=ORIENTED_EDGE('',*,*,#2350,.T.);
#3085=ORIENTED_EDGE('',*,*,#2358,.T.);
#3086=ORIENTED_EDGE('',*,*,#2356,.T.);
#3087=ORIENTED_EDGE('',*,*,#2358,.F.);
#3088=ORIENTED_EDGE('',*,*,#2357,.T.);
#3089=ORIENTED_EDGE('',*,*,#2359,.T.);
#3090=ORIENTED_EDGE('',*,*,#2360,.T.);
#3091=ORIENTED_EDGE('',*,*,#2359,.F.);
#3092=ORIENTED_EDGE('',*,*,#2361,.F.);
#3093=ORIENTED_EDGE('',*,*,#2362,.T.);
#3094=ORIENTED_EDGE('',*,*,#2363,.T.);
#3095=ORIENTED_EDGE('',*,*,#2362,.F.);
#3096=ORIENTED_EDGE('',*,*,#2364,.F.);
#3097=ORIENTED_EDGE('',*,*,#2365,.T.);
#3098=ORIENTED_EDGE('',*,*,#2355,.T.);
#3099=ORIENTED_EDGE('',*,*,#2365,.F.);
#3100=ORIENTED_EDGE('',*,*,#2364,.T.);
#3101=ORIENTED_EDGE('',*,*,#2361,.T.);
#3102=ORIENTED_EDGE('',*,*,#2347,.T.);
#3103=ORIENTED_EDGE('',*,*,#2344,.T.);
#3104=ORIENTED_EDGE('',*,*,#2341,.T.);
#3105=ORIENTED_EDGE('',*,*,#2338,.T.);
#3106=ORIENTED_EDGE('',*,*,#2360,.F.);
#3107=ORIENTED_EDGE('',*,*,#2363,.F.);
#3108=ORIENTED_EDGE('',*,*,#2345,.T.);
#3109=ORIENTED_EDGE('',*,*,#2342,.T.);
#3110=ORIENTED_EDGE('',*,*,#2339,.T.);
#3111=ORIENTED_EDGE('',*,*,#2336,.T.);
#3112=ORIENTED_EDGE('',*,*,#2366,.F.);
#3113=ORIENTED_EDGE('',*,*,#2367,.T.);
#3114=ORIENTED_EDGE('',*,*,#2368,.T.);
#3115=ORIENTED_EDGE('',*,*,#2367,.F.);
#3116=ORIENTED_EDGE('',*,*,#2369,.F.);
#3117=ORIENTED_EDGE('',*,*,#2370,.T.);
#3118=ORIENTED_EDGE('',*,*,#2371,.T.);
#3119=ORIENTED_EDGE('',*,*,#2370,.F.);
#3120=ORIENTED_EDGE('',*,*,#2369,.T.);
#3121=ORIENTED_EDGE('',*,*,#2366,.T.);
#3122=ORIENTED_EDGE('',*,*,#2371,.F.);
#3123=ORIENTED_EDGE('',*,*,#2368,.F.);
#3124=ORIENTED_EDGE('',*,*,#2372,.F.);
#3125=ORIENTED_EDGE('',*,*,#2373,.F.);
#3126=ORIENTED_EDGE('',*,*,#2374,.T.);
#3127=ORIENTED_EDGE('',*,*,#2375,.F.);
#3128=ORIENTED_EDGE('',*,*,#2376,.F.);
#3129=ORIENTED_EDGE('',*,*,#2374,.F.);
#3130=ORIENTED_EDGE('',*,*,#2375,.T.);
#3131=ORIENTED_EDGE('',*,*,#2376,.T.);
#3132=ORIENTED_EDGE('',*,*,#2377,.T.);
#3133=ORIENTED_EDGE('',*,*,#2378,.T.);
#3134=ORIENTED_EDGE('',*,*,#2377,.F.);
#3135=ORIENTED_EDGE('',*,*,#2379,.T.);
#3136=ORIENTED_EDGE('',*,*,#2380,.T.);
#3137=ORIENTED_EDGE('',*,*,#2381,.F.);
#3138=ORIENTED_EDGE('',*,*,#2380,.F.);
#3139=ORIENTED_EDGE('',*,*,#2381,.T.);
#3140=ORIENTED_EDGE('',*,*,#2382,.T.);
#3141=ORIENTED_EDGE('',*,*,#2383,.F.);
#3142=ORIENTED_EDGE('',*,*,#2382,.F.);
#3143=ORIENTED_EDGE('',*,*,#2378,.F.);
#3144=ORIENTED_EDGE('',*,*,#2383,.T.);
#3145=ORIENTED_EDGE('',*,*,#2384,.F.);
#3146=ORIENTED_EDGE('',*,*,#2385,.T.);
#3147=ORIENTED_EDGE('',*,*,#2372,.T.);
#3148=ORIENTED_EDGE('',*,*,#2373,.T.);
#3149=ORIENTED_EDGE('',*,*,#2385,.F.);
#3150=ORIENTED_EDGE('',*,*,#2384,.T.);
#3151=ORIENTED_EDGE('',*,*,#2386,.F.);
#3152=ORIENTED_EDGE('',*,*,#2386,.T.);
#3153=ORIENTED_EDGE('',*,*,#2387,.T.);
#3154=ORIENTED_EDGE('',*,*,#2379,.F.);
#3155=ORIENTED_EDGE('',*,*,#2387,.F.);
#3156=ORIENTED_EDGE('',*,*,#2388,.F.);
#3157=ORIENTED_EDGE('',*,*,#2389,.F.);
#3158=ORIENTED_EDGE('',*,*,#2390,.T.);
#3159=ORIENTED_EDGE('',*,*,#2391,.F.);
#3160=ORIENTED_EDGE('',*,*,#2392,.F.);
#3161=ORIENTED_EDGE('',*,*,#2390,.F.);
#3162=ORIENTED_EDGE('',*,*,#2393,.T.);
#3163=ORIENTED_EDGE('',*,*,#2394,.T.);
#3164=ORIENTED_EDGE('',*,*,#2391,.T.);
#3165=ORIENTED_EDGE('',*,*,#2392,.T.);
#3166=ORIENTED_EDGE('',*,*,#2394,.F.);
#3167=ORIENTED_EDGE('',*,*,#2395,.F.);
#3168=ORIENTED_EDGE('',*,*,#2396,.T.);
#3169=ORIENTED_EDGE('',*,*,#2397,.F.);
#3170=ORIENTED_EDGE('',*,*,#2398,.T.);
#3171=ORIENTED_EDGE('',*,*,#2395,.T.);
#3172=ORIENTED_EDGE('',*,*,#2398,.F.);
#3173=ORIENTED_EDGE('',*,*,#2399,.F.);
#3174=ORIENTED_EDGE('',*,*,#2400,.T.);
#3175=ORIENTED_EDGE('',*,*,#2397,.T.);
#3176=ORIENTED_EDGE('',*,*,#2400,.F.);
#3177=ORIENTED_EDGE('',*,*,#2401,.F.);
#3178=ORIENTED_EDGE('',*,*,#2402,.T.);
#3179=ORIENTED_EDGE('',*,*,#2399,.T.);
#3180=ORIENTED_EDGE('',*,*,#2402,.F.);
#3181=ORIENTED_EDGE('',*,*,#2401,.T.);
#3182=ORIENTED_EDGE('',*,*,#2393,.F.);
#3183=ORIENTED_EDGE('',*,*,#2388,.T.);
#3184=ORIENTED_EDGE('',*,*,#2389,.T.);
#3185=ORIENTED_EDGE('',*,*,#2403,.T.);
#3186=ORIENTED_EDGE('',*,*,#2396,.F.);
#3187=ORIENTED_EDGE('',*,*,#2403,.F.);
#3188=ORIENTED_EDGE('',*,*,#2404,.T.);
#3189=ORIENTED_EDGE('',*,*,#2404,.F.);
#3190=ORIENTED_EDGE('',*,*,#2405,.T.);
#3191=ORIENTED_EDGE('',*,*,#2405,.F.);
#3192=ORIENTED_EDGE('',*,*,#2406,.T.);
#3193=ORIENTED_EDGE('',*,*,#2406,.F.);
#3194=ORIENTED_EDGE('',*,*,#2407,.T.);
#3195=ORIENTED_EDGE('',*,*,#2407,.F.);
#3196=ORIENTED_EDGE('',*,*,#2408,.T.);
#3197=ORIENTED_EDGE('',*,*,#2408,.F.);
#3198=ORIENTED_EDGE('',*,*,#2409,.T.);
#3199=ORIENTED_EDGE('',*,*,#2409,.F.);
#3200=ORIENTED_EDGE('',*,*,#2410,.T.);
#3201=ORIENTED_EDGE('',*,*,#2410,.F.);
#3202=ORIENTED_EDGE('',*,*,#2411,.T.);
#3203=ORIENTED_EDGE('',*,*,#2411,.F.);
#3204=ORIENTED_EDGE('',*,*,#2412,.F.);
#3205=ORIENTED_EDGE('',*,*,#2413,.F.);
#3206=ORIENTED_EDGE('',*,*,#2414,.F.);
#3207=ORIENTED_EDGE('',*,*,#2415,.F.);
#3208=ORIENTED_EDGE('',*,*,#2414,.T.);
#3209=ORIENTED_EDGE('',*,*,#2416,.F.);
#3210=ORIENTED_EDGE('',*,*,#2417,.T.);
#3211=ORIENTED_EDGE('',*,*,#2418,.F.);
#3212=ORIENTED_EDGE('',*,*,#2419,.T.);
#3213=ORIENTED_EDGE('',*,*,#2420,.F.);
#3214=ORIENTED_EDGE('',*,*,#2421,.T.);
#3215=ORIENTED_EDGE('',*,*,#2422,.T.);
#3216=ORIENTED_EDGE('',*,*,#2423,.F.);
#3217=ORIENTED_EDGE('',*,*,#2422,.F.);
#3218=ORIENTED_EDGE('',*,*,#2424,.T.);
#3219=ORIENTED_EDGE('',*,*,#2425,.F.);
#3220=ORIENTED_EDGE('',*,*,#2426,.T.);
#3221=ORIENTED_EDGE('',*,*,#2427,.F.);
#3222=ORIENTED_EDGE('',*,*,#2428,.T.);
#3223=ORIENTED_EDGE('',*,*,#2429,.F.);
#3224=ORIENTED_EDGE('',*,*,#2430,.T.);
#3225=ORIENTED_EDGE('',*,*,#2431,.F.);
#3226=ORIENTED_EDGE('',*,*,#2432,.T.);
#3227=ORIENTED_EDGE('',*,*,#2433,.F.);
#3228=ORIENTED_EDGE('',*,*,#2413,.T.);
#3229=ORIENTED_EDGE('',*,*,#2434,.T.);
#3230=ORIENTED_EDGE('',*,*,#2435,.T.);
#3231=ORIENTED_EDGE('',*,*,#2416,.T.);
#3232=ORIENTED_EDGE('',*,*,#2436,.F.);
#3233=ORIENTED_EDGE('',*,*,#2437,.F.);
#3234=ORIENTED_EDGE('',*,*,#2417,.F.);
#3235=ORIENTED_EDGE('',*,*,#2435,.F.);
#3236=ORIENTED_EDGE('',*,*,#2437,.T.);
#3237=ORIENTED_EDGE('',*,*,#2438,.T.);
#3238=ORIENTED_EDGE('',*,*,#2439,.T.);
#3239=ORIENTED_EDGE('',*,*,#2418,.T.);
#3240=ORIENTED_EDGE('',*,*,#2440,.F.);
#3241=ORIENTED_EDGE('',*,*,#2441,.F.);
#3242=ORIENTED_EDGE('',*,*,#2419,.F.);
#3243=ORIENTED_EDGE('',*,*,#2439,.F.);
#3244=ORIENTED_EDGE('',*,*,#2441,.T.);
#3245=ORIENTED_EDGE('',*,*,#2442,.T.);
#3246=ORIENTED_EDGE('',*,*,#2443,.T.);
#3247=ORIENTED_EDGE('',*,*,#2420,.T.);
#3248=ORIENTED_EDGE('',*,*,#2444,.F.);
#3249=ORIENTED_EDGE('',*,*,#2445,.F.);
#3250=ORIENTED_EDGE('',*,*,#2424,.F.);
#3251=ORIENTED_EDGE('',*,*,#2421,.F.);
#3252=ORIENTED_EDGE('',*,*,#2443,.F.);
#3253=ORIENTED_EDGE('',*,*,#2446,.F.);
#3254=ORIENTED_EDGE('',*,*,#2445,.T.);
#3255=ORIENTED_EDGE('',*,*,#2447,.T.);
#3256=ORIENTED_EDGE('',*,*,#2448,.T.);
#3257=ORIENTED_EDGE('',*,*,#2425,.T.);
#3258=ORIENTED_EDGE('',*,*,#2449,.F.);
#3259=ORIENTED_EDGE('',*,*,#2450,.F.);
#3260=ORIENTED_EDGE('',*,*,#2426,.F.);
#3261=ORIENTED_EDGE('',*,*,#2448,.F.);
#3262=ORIENTED_EDGE('',*,*,#2450,.T.);
#3263=ORIENTED_EDGE('',*,*,#2451,.T.);
#3264=ORIENTED_EDGE('',*,*,#2452,.T.);
#3265=ORIENTED_EDGE('',*,*,#2427,.T.);
#3266=ORIENTED_EDGE('',*,*,#2453,.F.);
#3267=ORIENTED_EDGE('',*,*,#2454,.F.);
#3268=ORIENTED_EDGE('',*,*,#2428,.F.);
#3269=ORIENTED_EDGE('',*,*,#2452,.F.);
#3270=ORIENTED_EDGE('',*,*,#2454,.T.);
#3271=ORIENTED_EDGE('',*,*,#2455,.T.);
#3272=ORIENTED_EDGE('',*,*,#2456,.T.);
#3273=ORIENTED_EDGE('',*,*,#2429,.T.);
#3274=ORIENTED_EDGE('',*,*,#2430,.F.);
#3275=ORIENTED_EDGE('',*,*,#2456,.F.);
#3276=ORIENTED_EDGE('',*,*,#2457,.F.);
#3277=ORIENTED_EDGE('',*,*,#2458,.F.);
#3278=ORIENTED_EDGE('',*,*,#2459,.F.);
#3279=ORIENTED_EDGE('',*,*,#2460,.T.);
#3280=ORIENTED_EDGE('',*,*,#2446,.T.);
#3281=ORIENTED_EDGE('',*,*,#2442,.F.);
#3282=ORIENTED_EDGE('',*,*,#2440,.T.);
#3283=ORIENTED_EDGE('',*,*,#2438,.F.);
#3284=ORIENTED_EDGE('',*,*,#2436,.T.);
#3285=ORIENTED_EDGE('',*,*,#2434,.F.);
#3286=ORIENTED_EDGE('',*,*,#2412,.T.);
#3287=ORIENTED_EDGE('',*,*,#2461,.F.);
#3288=ORIENTED_EDGE('',*,*,#2462,.T.);
#3289=ORIENTED_EDGE('',*,*,#2463,.F.);
#3290=ORIENTED_EDGE('',*,*,#2457,.T.);
#3291=ORIENTED_EDGE('',*,*,#2455,.F.);
#3292=ORIENTED_EDGE('',*,*,#2453,.T.);
#3293=ORIENTED_EDGE('',*,*,#2451,.F.);
#3294=ORIENTED_EDGE('',*,*,#2449,.T.);
#3295=ORIENTED_EDGE('',*,*,#2447,.F.);
#3296=ORIENTED_EDGE('',*,*,#2444,.T.);
#3297=ORIENTED_EDGE('',*,*,#2460,.F.);
#3298=ORIENTED_EDGE('',*,*,#2415,.T.);
#3299=ORIENTED_EDGE('',*,*,#2433,.T.);
#3300=ORIENTED_EDGE('',*,*,#2464,.T.);
#3301=ORIENTED_EDGE('',*,*,#2461,.T.);
#3302=ORIENTED_EDGE('',*,*,#2432,.F.);
#3303=ORIENTED_EDGE('',*,*,#2465,.F.);
#3304=ORIENTED_EDGE('',*,*,#2462,.F.);
#3305=ORIENTED_EDGE('',*,*,#2464,.F.);
#3306=ORIENTED_EDGE('',*,*,#2423,.T.);
#3307=ORIENTED_EDGE('',*,*,#2459,.T.);
#3308=ORIENTED_EDGE('',*,*,#2458,.T.);
#3309=ORIENTED_EDGE('',*,*,#2463,.T.);
#3310=ORIENTED_EDGE('',*,*,#2465,.T.);
#3311=ORIENTED_EDGE('',*,*,#2431,.T.);
#3312=ORIENTED_EDGE('',*,*,#2466,.F.);
#3313=ORIENTED_EDGE('',*,*,#2467,.T.);
#3314=ORIENTED_EDGE('',*,*,#2468,.F.);
#3315=ORIENTED_EDGE('',*,*,#2469,.T.);
#3316=ORIENTED_EDGE('',*,*,#2466,.T.);
#3317=ORIENTED_EDGE('',*,*,#2469,.F.);
#3318=ORIENTED_EDGE('',*,*,#2468,.T.);
#3319=ORIENTED_EDGE('',*,*,#2470,.F.);
#3320=ORIENTED_EDGE('',*,*,#2470,.T.);
#3321=ORIENTED_EDGE('',*,*,#2471,.T.);
#3322=ORIENTED_EDGE('',*,*,#2467,.F.);
#3323=ORIENTED_EDGE('',*,*,#2471,.F.);
#3324=ORIENTED_EDGE('',*,*,#2472,.F.);
#3325=ORIENTED_EDGE('',*,*,#2473,.T.);
#3326=ORIENTED_EDGE('',*,*,#2474,.F.);
#3327=ORIENTED_EDGE('',*,*,#2475,.T.);
#3328=ORIENTED_EDGE('',*,*,#2472,.T.);
#3329=ORIENTED_EDGE('',*,*,#2475,.F.);
#3330=ORIENTED_EDGE('',*,*,#2474,.T.);
#3331=ORIENTED_EDGE('',*,*,#2476,.F.);
#3332=ORIENTED_EDGE('',*,*,#2476,.T.);
#3333=ORIENTED_EDGE('',*,*,#2477,.T.);
#3334=ORIENTED_EDGE('',*,*,#2473,.F.);
#3335=ORIENTED_EDGE('',*,*,#2477,.F.);
#3336=ORIENTED_EDGE('',*,*,#2478,.F.);
#3337=ORIENTED_EDGE('',*,*,#2479,.T.);
#3338=ORIENTED_EDGE('',*,*,#2480,.F.);
#3339=ORIENTED_EDGE('',*,*,#2479,.F.);
#3340=ORIENTED_EDGE('',*,*,#2481,.F.);
#3341=ORIENTED_EDGE('',*,*,#2482,.T.);
#3342=ORIENTED_EDGE('',*,*,#2483,.F.);
#3343=ORIENTED_EDGE('',*,*,#2482,.F.);
#3344=ORIENTED_EDGE('',*,*,#2484,.F.);
#3345=ORIENTED_EDGE('',*,*,#2485,.T.);
#3346=ORIENTED_EDGE('',*,*,#2486,.F.);
#3347=ORIENTED_EDGE('',*,*,#2485,.F.);
#3348=ORIENTED_EDGE('',*,*,#2487,.F.);
#3349=ORIENTED_EDGE('',*,*,#2488,.T.);
#3350=ORIENTED_EDGE('',*,*,#2489,.F.);
#3351=ORIENTED_EDGE('',*,*,#2488,.F.);
#3352=ORIENTED_EDGE('',*,*,#2490,.F.);
#3353=ORIENTED_EDGE('',*,*,#2491,.T.);
#3354=ORIENTED_EDGE('',*,*,#2492,.F.);
#3355=ORIENTED_EDGE('',*,*,#2491,.F.);
#3356=ORIENTED_EDGE('',*,*,#2490,.T.);
#3357=ORIENTED_EDGE('',*,*,#2493,.T.);
#3358=ORIENTED_EDGE('',*,*,#2493,.F.);
#3359=ORIENTED_EDGE('',*,*,#2494,.T.);
#3360=ORIENTED_EDGE('',*,*,#2495,.T.);
#3361=ORIENTED_EDGE('',*,*,#2494,.F.);
#3362=ORIENTED_EDGE('',*,*,#2496,.F.);
#3363=ORIENTED_EDGE('',*,*,#2497,.T.);
#3364=ORIENTED_EDGE('',*,*,#2498,.T.);
#3365=ORIENTED_EDGE('',*,*,#2497,.F.);
#3366=ORIENTED_EDGE('',*,*,#2496,.T.);
#3367=ORIENTED_EDGE('',*,*,#2492,.T.);
#3368=ORIENTED_EDGE('',*,*,#2489,.T.);
#3369=ORIENTED_EDGE('',*,*,#2486,.T.);
#3370=ORIENTED_EDGE('',*,*,#2483,.T.);
#3371=ORIENTED_EDGE('',*,*,#2480,.T.);
#3372=ORIENTED_EDGE('',*,*,#2498,.F.);
#3373=ORIENTED_EDGE('',*,*,#2495,.F.);
#3374=ORIENTED_EDGE('',*,*,#2487,.T.);
#3375=ORIENTED_EDGE('',*,*,#2484,.T.);
#3376=ORIENTED_EDGE('',*,*,#2481,.T.);
#3377=ORIENTED_EDGE('',*,*,#2478,.T.);
#3378=ORIENTED_EDGE('',*,*,#2499,.T.);
#3379=ORIENTED_EDGE('',*,*,#2500,.T.);
#3380=ORIENTED_EDGE('',*,*,#2501,.T.);
#3381=ORIENTED_EDGE('',*,*,#2502,.F.);
#3382=ORIENTED_EDGE('',*,*,#2503,.T.);
#3383=ORIENTED_EDGE('',*,*,#2504,.T.);
#3384=ORIENTED_EDGE('',*,*,#2505,.T.);
#3385=ORIENTED_EDGE('',*,*,#2500,.F.);
#3386=ORIENTED_EDGE('',*,*,#2506,.T.);
#3387=ORIENTED_EDGE('',*,*,#2507,.T.);
#3388=ORIENTED_EDGE('',*,*,#2508,.T.);
#3389=ORIENTED_EDGE('',*,*,#2504,.F.);
#3390=ORIENTED_EDGE('',*,*,#2509,.T.);
#3391=ORIENTED_EDGE('',*,*,#2510,.T.);
#3392=ORIENTED_EDGE('',*,*,#2511,.T.);
#3393=ORIENTED_EDGE('',*,*,#2507,.F.);
#3394=ORIENTED_EDGE('',*,*,#2512,.T.);
#3395=ORIENTED_EDGE('',*,*,#2513,.T.);
#3396=ORIENTED_EDGE('',*,*,#2514,.T.);
#3397=ORIENTED_EDGE('',*,*,#2510,.F.);
#3398=ORIENTED_EDGE('',*,*,#2515,.T.);
#3399=ORIENTED_EDGE('',*,*,#2502,.T.);
#3400=ORIENTED_EDGE('',*,*,#2516,.T.);
#3401=ORIENTED_EDGE('',*,*,#2513,.F.);
#3402=ORIENTED_EDGE('',*,*,#2515,.F.);
#3403=ORIENTED_EDGE('',*,*,#2512,.F.);
#3404=ORIENTED_EDGE('',*,*,#2509,.F.);
#3405=ORIENTED_EDGE('',*,*,#2506,.F.);
#3406=ORIENTED_EDGE('',*,*,#2503,.F.);
#3407=ORIENTED_EDGE('',*,*,#2499,.F.);
#3408=ORIENTED_EDGE('',*,*,#2516,.F.);
#3409=ORIENTED_EDGE('',*,*,#2501,.F.);
#3410=ORIENTED_EDGE('',*,*,#2505,.F.);
#3411=ORIENTED_EDGE('',*,*,#2508,.F.);
#3412=ORIENTED_EDGE('',*,*,#2511,.F.);
#3413=ORIENTED_EDGE('',*,*,#2514,.F.);
#3414=ORIENTED_EDGE('',*,*,#2517,.F.);
#3415=ORIENTED_EDGE('',*,*,#2518,.F.);
#3416=ORIENTED_EDGE('',*,*,#2519,.F.);
#3417=ORIENTED_EDGE('',*,*,#2520,.T.);
#3418=ORIENTED_EDGE('',*,*,#2518,.T.);
#3419=ORIENTED_EDGE('',*,*,#2520,.F.);
#3420=ORIENTED_EDGE('',*,*,#2521,.F.);
#3421=ORIENTED_EDGE('',*,*,#2522,.T.);
#3422=ORIENTED_EDGE('',*,*,#2519,.T.);
#3423=ORIENTED_EDGE('',*,*,#2522,.F.);
#3424=ORIENTED_EDGE('',*,*,#2523,.F.);
#3425=ORIENTED_EDGE('',*,*,#2524,.T.);
#3426=ORIENTED_EDGE('',*,*,#2521,.T.);
#3427=ORIENTED_EDGE('',*,*,#2524,.F.);
#3428=ORIENTED_EDGE('',*,*,#2523,.T.);
#3429=ORIENTED_EDGE('',*,*,#2525,.F.);
#3430=ORIENTED_EDGE('',*,*,#2526,.F.);
#3431=ORIENTED_EDGE('',*,*,#2527,.T.);
#3432=ORIENTED_EDGE('',*,*,#2525,.T.);
#3433=ORIENTED_EDGE('',*,*,#2527,.F.);
#3434=ORIENTED_EDGE('',*,*,#2517,.T.);
#3435=ORIENTED_EDGE('',*,*,#2528,.T.);
#3436=ORIENTED_EDGE('',*,*,#2526,.T.);
#3437=ORIENTED_EDGE('',*,*,#2528,.F.);
#3438=ORIENTED_EDGE('',*,*,#2529,.T.);
#3439=ORIENTED_EDGE('',*,*,#2530,.F.);
#3440=ORIENTED_EDGE('',*,*,#2531,.F.);
#3441=ORIENTED_EDGE('',*,*,#2532,.F.);
#3442=ORIENTED_EDGE('',*,*,#2529,.F.);
#3443=ORIENTED_EDGE('',*,*,#2533,.T.);
#3444=ORIENTED_EDGE('',*,*,#2531,.T.);
#3445=ORIENTED_EDGE('',*,*,#2533,.F.);
#3446=ORIENTED_EDGE('',*,*,#2532,.T.);
#3447=ORIENTED_EDGE('',*,*,#2534,.T.);
#3448=ORIENTED_EDGE('',*,*,#2535,.F.);
#3449=ORIENTED_EDGE('',*,*,#2536,.F.);
#3450=ORIENTED_EDGE('',*,*,#2537,.F.);
#3451=ORIENTED_EDGE('',*,*,#2534,.F.);
#3452=ORIENTED_EDGE('',*,*,#2538,.F.);
#3453=ORIENTED_EDGE('',*,*,#2539,.T.);
#3454=ORIENTED_EDGE('',*,*,#2530,.T.);
#3455=ORIENTED_EDGE('',*,*,#2539,.F.);
#3456=ORIENTED_EDGE('',*,*,#2538,.T.);
#3457=ORIENTED_EDGE('',*,*,#2536,.T.);
#3458=ORIENTED_EDGE('',*,*,#2540,.F.);
#3459=ORIENTED_EDGE('',*,*,#2541,.T.);
#3460=ORIENTED_EDGE('',*,*,#2542,.F.);
#3461=ORIENTED_EDGE('',*,*,#2535,.T.);
#3462=ORIENTED_EDGE('',*,*,#2537,.T.);
#3463=ORIENTED_EDGE('',*,*,#2543,.F.);
#3464=ORIENTED_EDGE('',*,*,#2544,.F.);
#3465=ORIENTED_EDGE('',*,*,#2545,.F.);
#3466=ORIENTED_EDGE('',*,*,#2546,.F.);
#3467=ORIENTED_EDGE('',*,*,#2547,.F.);
#3468=ORIENTED_EDGE('',*,*,#2544,.T.);
#3469=ORIENTED_EDGE('',*,*,#2548,.F.);
#3470=ORIENTED_EDGE('',*,*,#2549,.F.);
#3471=ORIENTED_EDGE('',*,*,#2550,.F.);
#3472=ORIENTED_EDGE('',*,*,#2551,.F.);
#3473=ORIENTED_EDGE('',*,*,#2552,.F.);
#3474=ORIENTED_EDGE('',*,*,#2553,.T.);
#3475=ORIENTED_EDGE('',*,*,#2550,.T.);
#3476=ORIENTED_EDGE('',*,*,#2554,.T.);
#3477=ORIENTED_EDGE('',*,*,#2555,.T.);
#3478=ORIENTED_EDGE('',*,*,#2556,.T.);
#3479=ORIENTED_EDGE('',*,*,#2548,.T.);
#3480=ORIENTED_EDGE('',*,*,#2543,.T.);
#3481=ORIENTED_EDGE('',*,*,#2542,.T.);
#3482=ORIENTED_EDGE('',*,*,#2549,.T.);
#3483=ORIENTED_EDGE('',*,*,#2557,.T.);
#3484=ORIENTED_EDGE('',*,*,#2558,.T.);
#3485=ORIENTED_EDGE('',*,*,#2554,.F.);
#3486=ORIENTED_EDGE('',*,*,#2559,.T.);
#3487=ORIENTED_EDGE('',*,*,#2540,.T.);
#3488=ORIENTED_EDGE('',*,*,#2545,.T.);
#3489=ORIENTED_EDGE('',*,*,#2547,.T.);
#3490=ORIENTED_EDGE('',*,*,#2560,.F.);
#3491=ORIENTED_EDGE('',*,*,#2561,.T.);
#3492=ORIENTED_EDGE('',*,*,#2557,.F.);
#3493=ORIENTED_EDGE('',*,*,#2552,.T.);
#3494=ORIENTED_EDGE('',*,*,#2559,.F.);
#3495=ORIENTED_EDGE('',*,*,#2551,.T.);
#3496=ORIENTED_EDGE('',*,*,#2553,.F.);
#3497=ORIENTED_EDGE('',*,*,#2541,.F.);
#3498=ORIENTED_EDGE('',*,*,#2562,.F.);
#3499=ORIENTED_EDGE('',*,*,#2555,.F.);
#3500=ORIENTED_EDGE('',*,*,#2558,.F.);
#3501=ORIENTED_EDGE('',*,*,#2561,.F.);
#3502=ORIENTED_EDGE('',*,*,#2546,.T.);
#3503=ORIENTED_EDGE('',*,*,#2556,.F.);
#3504=ORIENTED_EDGE('',*,*,#2562,.T.);
#3505=ORIENTED_EDGE('',*,*,#2560,.T.);
#3506=ORIENTED_EDGE('',*,*,#2563,.F.);
#3507=ORIENTED_EDGE('',*,*,#2564,.T.);
#3508=ORIENTED_EDGE('',*,*,#2565,.T.);
#3509=ORIENTED_EDGE('',*,*,#2564,.F.);
#3510=ORIENTED_EDGE('',*,*,#2566,.F.);
#3511=ORIENTED_EDGE('',*,*,#2567,.T.);
#3512=ORIENTED_EDGE('',*,*,#2568,.T.);
#3513=ORIENTED_EDGE('',*,*,#2567,.F.);
#3514=ORIENTED_EDGE('',*,*,#2566,.T.);
#3515=ORIENTED_EDGE('',*,*,#2563,.T.);
#3516=ORIENTED_EDGE('',*,*,#2568,.F.);
#3517=ORIENTED_EDGE('',*,*,#2565,.F.);
#3518=ORIENTED_EDGE('',*,*,#2569,.F.);
#3519=ORIENTED_EDGE('',*,*,#2570,.T.);
#3520=ORIENTED_EDGE('',*,*,#2571,.F.);
#3521=ORIENTED_EDGE('',*,*,#2570,.F.);
#3522=ORIENTED_EDGE('',*,*,#2572,.T.);
#3523=ORIENTED_EDGE('',*,*,#2573,.T.);
#3524=ORIENTED_EDGE('',*,*,#2574,.F.);
#3525=ORIENTED_EDGE('',*,*,#2575,.F.);
#3526=ORIENTED_EDGE('',*,*,#2576,.T.);
#3527=ORIENTED_EDGE('',*,*,#2575,.T.);
#3528=ORIENTED_EDGE('',*,*,#2577,.F.);
#3529=ORIENTED_EDGE('',*,*,#2578,.F.);
#3530=ORIENTED_EDGE('',*,*,#2579,.T.);
#3531=ORIENTED_EDGE('',*,*,#2578,.T.);
#3532=ORIENTED_EDGE('',*,*,#2580,.F.);
#3533=ORIENTED_EDGE('',*,*,#2581,.F.);
#3534=ORIENTED_EDGE('',*,*,#2582,.T.);
#3535=ORIENTED_EDGE('',*,*,#2581,.T.);
#3536=ORIENTED_EDGE('',*,*,#2583,.F.);
#3537=ORIENTED_EDGE('',*,*,#2584,.F.);
#3538=ORIENTED_EDGE('',*,*,#2585,.T.);
#3539=ORIENTED_EDGE('',*,*,#2584,.T.);
#3540=ORIENTED_EDGE('',*,*,#2586,.F.);
#3541=ORIENTED_EDGE('',*,*,#2587,.F.);
#3542=ORIENTED_EDGE('',*,*,#2588,.T.);
#3543=ORIENTED_EDGE('',*,*,#2587,.T.);
#3544=ORIENTED_EDGE('',*,*,#2589,.F.);
#3545=ORIENTED_EDGE('',*,*,#2573,.F.);
#3546=ORIENTED_EDGE('',*,*,#2589,.T.);
#3547=ORIENTED_EDGE('',*,*,#2586,.T.);
#3548=ORIENTED_EDGE('',*,*,#2583,.T.);
#3549=ORIENTED_EDGE('',*,*,#2580,.T.);
#3550=ORIENTED_EDGE('',*,*,#2577,.T.);
#3551=ORIENTED_EDGE('',*,*,#2574,.T.);
#3552=ORIENTED_EDGE('',*,*,#2571,.T.);
#3553=ORIENTED_EDGE('',*,*,#2588,.F.);
#3554=ORIENTED_EDGE('',*,*,#2572,.F.);
#3555=ORIENTED_EDGE('',*,*,#2576,.F.);
#3556=ORIENTED_EDGE('',*,*,#2579,.F.);
#3557=ORIENTED_EDGE('',*,*,#2582,.F.);
#3558=ORIENTED_EDGE('',*,*,#2585,.F.);
#3559=ORIENTED_EDGE('',*,*,#2569,.T.);
#3560=PLANE('',#4222);
#3561=PLANE('',#4254);
#3562=PLANE('',#4271);
#3563=PLANE('',#4272);
#3564=PLANE('',#4273);
#3565=PLANE('',#4274);
#3566=PLANE('',#4275);
#3567=PLANE('',#4276);
#3568=PLANE('',#4277);
#3569=PLANE('',#4278);
#3570=PLANE('',#4279);
#3571=PLANE('',#4280);
#3572=PLANE('',#4291);
#3573=PLANE('',#4292);
#3574=PLANE('',#4293);
#3575=PLANE('',#4294);
#3576=PLANE('',#4295);
#3577=PLANE('',#4296);
#3578=PLANE('',#4304);
#3579=PLANE('',#4305);
#3580=PLANE('',#4310);
#3581=PLANE('',#4311);
#3582=PLANE('',#4316);
#3583=PLANE('',#4319);
#3584=PLANE('',#4327);
#3585=PLANE('',#4328);
#3586=PLANE('',#4336);
#3587=PLANE('',#4337);
#3588=PLANE('',#4345);
#3589=PLANE('',#4346);
#3590=PLANE('',#4354);
#3591=PLANE('',#4355);
#3592=PLANE('',#4357);
#3593=PLANE('',#4358);
#3594=PLANE('',#4359);
#3595=PLANE('',#4360);
#3596=PLANE('',#4361);
#3597=PLANE('',#4362);
#3598=PLANE('',#4363);
#3599=PLANE('',#4364);
#3600=PLANE('',#4365);
#3601=PLANE('',#4370);
#3602=PLANE('',#4371);
#3603=PLANE('',#4379);
#3604=PLANE('',#4391);
#3605=PLANE('',#4392);
#3606=PLANE('',#4398);
#3607=PLANE('',#4399);
#3608=PLANE('',#4400);
#3609=PLANE('',#4404);
#3610=PLANE('',#4405);
#3611=PLANE('',#4406);
#3612=PLANE('',#4407);
#3613=PLANE('',#4408);
#3614=PLANE('',#4410);
#3615=PLANE('',#4418);
#3616=PLANE('',#4426);
#3617=PLANE('',#4427);
#3618=PLANE('',#4428);
#3619=PLANE('',#4429);
#3620=PLANE('',#4430);
#3621=PLANE('',#4431);
#3622=PLANE('',#4432);
#3623=PLANE('',#4433);
#3624=PLANE('',#4434);
#3625=PLANE('',#4479);
#3626=PLANE('',#4481);
#3627=PLANE('',#4492);
#3628=PLANE('',#4493);
#3629=PLANE('',#4501);
#3630=PLANE('',#4502);
#3631=PLANE('',#4518);
#3632=PLANE('',#4521);
#3633=PLANE('',#4533);
#3634=PLANE('',#4542);
#3635=PLANE('',#4575);
#3636=PLANE('',#4580);
#3637=PLANE('',#4585);
#3638=PLANE('',#4590);
#3639=PLANE('',#4595);
#3640=PLANE('',#4600);
#3641=PLANE('',#4609);
#3642=PLANE('',#4613);
#3643=PLANE('',#4614);
#3644=PLANE('',#4616);
#3645=PLANE('',#4621);
#3646=PLANE('',#4624);
#3647=PLANE('',#4629);
#3648=PLANE('',#4653);
#3649=PLANE('',#4660);
#3650=PLANE('',#4661);
#3651=PLANE('',#4663);
#3652=PLANE('',#4664);
#3653=PLANE('',#4665);
#3654=PLANE('',#4666);
#3655=PLANE('',#4667);
#3656=PLANE('',#4668);
#3657=PLANE('',#4669);
#3658=PLANE('',#4670);
#3659=PLANE('',#4671);
#3660=PLANE('',#4673);
#3661=PLANE('',#4681);
#3662=PLANE('',#4702);
#3663=PLANE('',#4705);
#3664=PLANE('',#4715);
#3665=PLANE('',#4716);
#3666=PLANE('',#4717);
#3667=PLANE('',#4718);
#3668=PLANE('',#4719);
#3669=PLANE('',#4720);
#3670=PLANE('',#4725);
#3671=PLANE('',#4727);
#3672=PLANE('',#4728);
#3673=PLANE('',#4737);
#3674=PLANE('',#4738);
#3675=PLANE('',#4743);
#3676=PLANE('',#4744);
#3677=PLANE('',#4745);
#3678=PLANE('',#4746);
#3679=PLANE('',#4747);
#3680=PLANE('',#4748);
#3681=PLANE('',#4749);
#3682=PLANE('',#4750);
#3683=ADVANCED_FACE('',(#1001,#921),#3560,.T.);
#3684=ADVANCED_FACE('',(#1002),#844,.F.);
#3685=ADVANCED_FACE('',(#1003),#845,.F.);
#3686=ADVANCED_FACE('',(#1004),#846,.F.);
#3687=ADVANCED_FACE('',(#1005),#847,.T.);
#3688=ADVANCED_FACE('',(#1006),#848,.F.);
#3689=ADVANCED_FACE('',(#1007),#849,.F.);
#3690=ADVANCED_FACE('',(#1008),#850,.F.);
#3691=ADVANCED_FACE('',(#1009),#851,.F.);
#3692=ADVANCED_FACE('',(#1010,#922),#3561,.T.);
#3693=ADVANCED_FACE('',(#1011),#852,.F.);
#3694=ADVANCED_FACE('',(#1012),#853,.F.);
#3695=ADVANCED_FACE('',(#1013),#854,.F.);
#3696=ADVANCED_FACE('',(#1014),#855,.F.);
#3697=ADVANCED_FACE('',(#1015),#856,.F.);
#3698=ADVANCED_FACE('',(#1016),#3562,.T.);
#3699=ADVANCED_FACE('',(#1017),#3563,.T.);
#3700=ADVANCED_FACE('',(#1018),#3564,.T.);
#3701=ADVANCED_FACE('',(#1019),#3565,.T.);
#3702=ADVANCED_FACE('',(#1020),#3566,.T.);
#3703=ADVANCED_FACE('',(#1021),#3567,.T.);
#3704=ADVANCED_FACE('',(#1022),#3568,.T.);
#3705=ADVANCED_FACE('',(#1023),#3569,.T.);
#3706=ADVANCED_FACE('',(#1024,#923,#924,#925,#926),#3570,.T.);
#3707=ADVANCED_FACE('',(#1025,#927,#928,#929,#930,#931,#932,#933,#934),
#3571,.F.);
#3708=ADVANCED_FACE('',(#1026),#857,.F.);
#3709=ADVANCED_FACE('',(#1027),#858,.F.);
#3710=ADVANCED_FACE('',(#1028),#859,.F.);
#3711=ADVANCED_FACE('',(#1029,#935,#936),#3572,.T.);
#3712=ADVANCED_FACE('',(#1030),#3573,.T.);
#3713=ADVANCED_FACE('',(#1031,#937,#938),#3574,.T.);
#3714=ADVANCED_FACE('',(#1032),#3575,.T.);
#3715=ADVANCED_FACE('',(#1033,#939),#3576,.T.);
#3716=ADVANCED_FACE('',(#1034,#940),#3577,.F.);
#3717=ADVANCED_FACE('',(#1035),#860,.F.);
#3718=ADVANCED_FACE('',(#1036),#861,.T.);
#3719=ADVANCED_FACE('',(#1037,#941),#3578,.T.);
#3720=ADVANCED_FACE('',(#1038,#942),#3579,.F.);
#3721=ADVANCED_FACE('',(#1039),#862,.F.);
#3722=ADVANCED_FACE('',(#1040),#3580,.T.);
#3723=ADVANCED_FACE('',(#1041,#943),#3581,.T.);
#3724=ADVANCED_FACE('',(#1042),#863,.T.);
#3725=ADVANCED_FACE('',(#1043),#3582,.F.);
#3726=ADVANCED_FACE('',(#1044),#864,.T.);
#3727=ADVANCED_FACE('',(#1045,#944),#3583,.T.);
#3728=ADVANCED_FACE('',(#1046),#865,.F.);
#3729=ADVANCED_FACE('',(#1047),#866,.T.);
#3730=ADVANCED_FACE('',(#1048,#945),#3584,.T.);
#3731=ADVANCED_FACE('',(#1049,#946),#3585,.F.);
#3732=ADVANCED_FACE('',(#1050),#867,.F.);
#3733=ADVANCED_FACE('',(#1051),#868,.T.);
#3734=ADVANCED_FACE('',(#1052,#947),#3586,.T.);
#3735=ADVANCED_FACE('',(#1053,#948),#3587,.F.);
#3736=ADVANCED_FACE('',(#1054),#869,.F.);
#3737=ADVANCED_FACE('',(#1055),#870,.T.);
#3738=ADVANCED_FACE('',(#1056,#949),#3588,.T.);
#3739=ADVANCED_FACE('',(#1057,#950),#3589,.F.);
#3740=ADVANCED_FACE('',(#1058),#871,.F.);
#3741=ADVANCED_FACE('',(#1059),#872,.T.);
#3742=ADVANCED_FACE('',(#1060,#951),#3590,.T.);
#3743=ADVANCED_FACE('',(#1061,#952),#3591,.F.);
#3744=ADVANCED_FACE('',(#1062),#3592,.F.);
#3745=ADVANCED_FACE('',(#1063),#3593,.F.);
#3746=ADVANCED_FACE('',(#1064),#3594,.F.);
#3747=ADVANCED_FACE('',(#1065),#3595,.F.);
#3748=ADVANCED_FACE('',(#1066),#3596,.F.);
#3749=ADVANCED_FACE('',(#1067),#3597,.F.);
#3750=ADVANCED_FACE('',(#1068),#3598,.F.);
#3751=ADVANCED_FACE('',(#1069),#3599,.F.);
#3752=ADVANCED_FACE('',(#1070,#953),#3600,.T.);
#3753=ADVANCED_FACE('',(#1071),#873,.T.);
#3754=ADVANCED_FACE('',(#1072),#3601,.F.);
#3755=ADVANCED_FACE('',(#1073),#3602,.T.);
#3756=ADVANCED_FACE('',(#1074),#251,.T.);
#3757=ADVANCED_FACE('',(#1075),#874,.T.);
#3758=ADVANCED_FACE('',(#1076),#252,.T.);
#3759=ADVANCED_FACE('',(#1077,#954),#3603,.T.);
#3760=ADVANCED_FACE('',(#1078),#253,.T.);
#3761=ADVANCED_FACE('',(#1079),#875,.T.);
#3762=ADVANCED_FACE('',(#1080),#876,.F.);
#3763=ADVANCED_FACE('',(#1081),#877,.T.);
#3764=ADVANCED_FACE('',(#1082,#955),#3604,.T.);
#3765=ADVANCED_FACE('',(#1083,#956),#3605,.F.);
#3766=ADVANCED_FACE('',(#1084),#254,.T.);
#3767=ADVANCED_FACE('',(#1085),#255,.T.);
#3768=ADVANCED_FACE('',(#1086),#3606,.T.);
#3769=ADVANCED_FACE('',(#1087),#3607,.T.);
#3770=ADVANCED_FACE('',(#1088),#3608,.T.);
#3771=ADVANCED_FACE('',(#1089),#878,.F.);
#3772=ADVANCED_FACE('',(#1090),#3609,.T.);
#3773=ADVANCED_FACE('',(#1091),#3610,.T.);
#3774=ADVANCED_FACE('',(#1092),#3611,.T.);
#3775=ADVANCED_FACE('',(#1093,#957),#3612,.T.);
#3776=ADVANCED_FACE('',(#1094,#958),#3613,.F.);
#3777=ADVANCED_FACE('',(#1095),#3614,.T.);
#3778=ADVANCED_FACE('',(#1096),#256,.T.);
#3779=ADVANCED_FACE('',(#1097),#879,.T.);
#3780=ADVANCED_FACE('',(#1098),#257,.T.);
#3781=ADVANCED_FACE('',(#1099,#959),#3615,.T.);
#3782=ADVANCED_FACE('',(#1100),#258,.T.);
#3783=ADVANCED_FACE('',(#1101),#880,.T.);
#3784=ADVANCED_FACE('',(#1102),#259,.T.);
#3785=ADVANCED_FACE('',(#1103),#3616,.T.);
#3786=ADVANCED_FACE('',(#1104),#3617,.F.);
#3787=ADVANCED_FACE('',(#1105),#3618,.F.);
#3788=ADVANCED_FACE('',(#1106),#3619,.F.);
#3789=ADVANCED_FACE('',(#1107),#3620,.F.);
#3790=ADVANCED_FACE('',(#1108),#3621,.F.);
#3791=ADVANCED_FACE('',(#1109),#3622,.F.);
#3792=ADVANCED_FACE('',(#1110),#3623,.F.);
#3793=ADVANCED_FACE('',(#1111),#3624,.F.);
#3794=ADVANCED_FACE('',(#1112),#881,.F.);
#3795=ADVANCED_FACE('',(#1113),#882,.F.);
#3796=ADVANCED_FACE('',(#1114),#883,.F.);
#3797=ADVANCED_FACE('',(#1115),#884,.F.);
#3798=ADVANCED_FACE('',(#1116),#260,.T.);
#3799=ADVANCED_FACE('',(#1117),#261,.T.);
#3800=ADVANCED_FACE('',(#1118),#885,.T.);
#3801=ADVANCED_FACE('',(#1119,#960),#3625,.T.);
#3802=ADVANCED_FACE('',(#1120,#961),#3626,.F.);
#3803=ADVANCED_FACE('',(#1121),#886,.T.);
#3804=ADVANCED_FACE('',(#1122),#887,.T.);
#3805=ADVANCED_FACE('',(#1123),#888,.F.);
#3806=ADVANCED_FACE('',(#1124),#889,.T.);
#3807=ADVANCED_FACE('',(#1125,#962,#963,#964,#965,#966),#3627,.T.);
#3808=ADVANCED_FACE('',(#1126,#967,#968,#969,#970,#971),#3628,.F.);
#3809=ADVANCED_FACE('',(#1127),#890,.F.);
#3810=ADVANCED_FACE('',(#1128),#891,.T.);
#3811=ADVANCED_FACE('',(#1129,#972),#3629,.T.);
#3812=ADVANCED_FACE('',(#1130,#973),#3630,.F.);
#3813=ADVANCED_FACE('',(#1131),#45,.F.);
#3814=ADVANCED_FACE('',(#1132),#892,.T.);
#3815=ADVANCED_FACE('',(#1133),#893,.F.);
#3816=ADVANCED_FACE('',(#1134),#262,.F.);
#3817=ADVANCED_FACE('',(#1135,#974),#3631,.T.);
#3818=ADVANCED_FACE('',(#1136),#894,.T.);
#3819=ADVANCED_FACE('',(#1137,#975),#3632,.T.);
#3820=ADVANCED_FACE('',(#1138),#263,.F.);
#3821=ADVANCED_FACE('',(#1139),#46,.F.);
#3822=ADVANCED_FACE('',(#1140),#895,.F.);
#3823=ADVANCED_FACE('',(#1141,#976),#3633,.T.);
#3824=ADVANCED_FACE('',(#1142),#264,.T.);
#3825=ADVANCED_FACE('',(#1143),#896,.T.);
#3826=ADVANCED_FACE('',(#1144),#265,.T.);
#3827=ADVANCED_FACE('',(#1145,#977),#3634,.T.);
#3828=ADVANCED_FACE('',(#1146),#897,.F.);
#3829=ADVANCED_FACE('',(#1147),#29,.T.);
#3830=ADVANCED_FACE('',(#1148),#30,.T.);
#3831=ADVANCED_FACE('',(#1149),#31,.T.);
#3832=ADVANCED_FACE('',(#1150),#32,.T.);
#3833=ADVANCED_FACE('',(#1151),#33,.T.);
#3834=ADVANCED_FACE('',(#1152),#34,.T.);
#3835=ADVANCED_FACE('',(#1153),#35,.T.);
#3836=ADVANCED_FACE('',(#1154),#36,.T.);
#3837=ADVANCED_FACE('',(#1155),#37,.F.);
#3838=ADVANCED_FACE('',(#1156),#898,.T.);
#3839=ADVANCED_FACE('',(#1157),#3635,.T.);
#3840=ADVANCED_FACE('',(#1158),#38,.F.);
#3841=ADVANCED_FACE('',(#1159),#3636,.T.);
#3842=ADVANCED_FACE('',(#1160),#39,.F.);
#3843=ADVANCED_FACE('',(#1161),#3637,.T.);
#3844=ADVANCED_FACE('',(#1162),#40,.F.);
#3845=ADVANCED_FACE('',(#1163),#3638,.T.);
#3846=ADVANCED_FACE('',(#1164),#41,.F.);
#3847=ADVANCED_FACE('',(#1165),#3639,.T.);
#3848=ADVANCED_FACE('',(#1166),#42,.F.);
#3849=ADVANCED_FACE('',(#1167),#3640,.T.);
#3850=ADVANCED_FACE('',(#1168),#43,.F.);
#3851=ADVANCED_FACE('',(#1169),#899,.F.);
#3852=ADVANCED_FACE('',(#1170),#3641,.T.);
#3853=ADVANCED_FACE('',(#1171),#44,.F.);
#3854=ADVANCED_FACE('',(#1172,#978),#3642,.T.);
#3855=ADVANCED_FACE('',(#1173),#3643,.T.);
#3856=ADVANCED_FACE('',(#1174,#979),#3644,.T.);
#3857=ADVANCED_FACE('',(#1175),#900,.T.);
#3858=ADVANCED_FACE('',(#1176,#980),#3645,.T.);
#3859=ADVANCED_FACE('',(#1177),#901,.F.);
#3860=ADVANCED_FACE('',(#1178,#981),#3646,.T.);
#3861=ADVANCED_FACE('',(#1179),#902,.T.);
#3862=ADVANCED_FACE('',(#1180,#982),#3647,.T.);
#3863=ADVANCED_FACE('',(#1181),#903,.F.);
#3864=ADVANCED_FACE('',(#1182),#904,.F.);
#3865=ADVANCED_FACE('',(#1183),#905,.F.);
#3866=ADVANCED_FACE('',(#1184),#906,.F.);
#3867=ADVANCED_FACE('',(#1185),#907,.F.);
#3868=ADVANCED_FACE('',(#1186),#908,.T.);
#3869=ADVANCED_FACE('',(#1187,#983),#3648,.T.);
#3870=ADVANCED_FACE('',(#1188),#909,.F.);
#3871=ADVANCED_FACE('',(#1189),#910,.T.);
#3872=ADVANCED_FACE('',(#1190,#984,#985,#986,#987,#988),#3649,.T.);
#3873=ADVANCED_FACE('',(#1191,#989,#990,#991,#992,#993),#3650,.F.);
#3874=ADVANCED_FACE('',(#1192),#3651,.F.);
#3875=ADVANCED_FACE('',(#1193),#3652,.F.);
#3876=ADVANCED_FACE('',(#1194),#3653,.F.);
#3877=ADVANCED_FACE('',(#1195),#3654,.F.);
#3878=ADVANCED_FACE('',(#1196),#3655,.F.);
#3879=ADVANCED_FACE('',(#1197),#3656,.F.);
#3880=ADVANCED_FACE('',(#1198),#3657,.F.);
#3881=ADVANCED_FACE('',(#1199),#3658,.F.);
#3882=ADVANCED_FACE('',(#1200),#3659,.F.);
#3883=ADVANCED_FACE('',(#1201),#3660,.T.);
#3884=ADVANCED_FACE('',(#1202),#266,.T.);
#3885=ADVANCED_FACE('',(#1203),#911,.T.);
#3886=ADVANCED_FACE('',(#1204),#267,.T.);
#3887=ADVANCED_FACE('',(#1205,#994),#3661,.T.);
#3888=ADVANCED_FACE('',(#1206),#268,.T.);
#3889=ADVANCED_FACE('',(#1207),#912,.T.);
#3890=ADVANCED_FACE('',(#1208,#995),#3662,.T.);
#3891=ADVANCED_FACE('',(#1209,#996),#3663,.F.);
#3892=ADVANCED_FACE('',(#1210),#913,.T.);
#3893=ADVANCED_FACE('',(#1211),#914,.T.);
#3894=ADVANCED_FACE('',(#1212),#915,.T.);
#3895=ADVANCED_FACE('',(#1213),#3664,.T.);
#3896=ADVANCED_FACE('',(#1214),#3665,.T.);
#3897=ADVANCED_FACE('',(#1215),#3666,.T.);
#3898=ADVANCED_FACE('',(#1216),#3667,.T.);
#3899=ADVANCED_FACE('',(#1217),#3668,.T.);
#3900=ADVANCED_FACE('',(#1218),#3669,.T.);
#3901=ADVANCED_FACE('',(#1219),#916,.F.);
#3902=ADVANCED_FACE('',(#1220),#3670,.F.);
#3903=ADVANCED_FACE('',(#1221),#3671,.F.);
#3904=ADVANCED_FACE('',(#1222),#3672,.F.);
#3905=ADVANCED_FACE('',(#1223),#917,.T.);
#3906=ADVANCED_FACE('',(#1224),#918,.F.);
#3907=ADVANCED_FACE('',(#1225),#919,.T.);
#3908=ADVANCED_FACE('',(#1226,#997),#3673,.T.);
#3909=ADVANCED_FACE('',(#1227,#998),#3674,.F.);
#3910=ADVANCED_FACE('',(#1228),#920,.F.);
#3911=ADVANCED_FACE('',(#1229),#3675,.T.);
#3912=ADVANCED_FACE('',(#1230),#3676,.T.);
#3913=ADVANCED_FACE('',(#1231),#3677,.T.);
#3914=ADVANCED_FACE('',(#1232),#3678,.T.);
#3915=ADVANCED_FACE('',(#1233),#3679,.T.);
#3916=ADVANCED_FACE('',(#1234),#3680,.T.);
#3917=ADVANCED_FACE('',(#1235,#999),#3681,.T.);
#3918=ADVANCED_FACE('',(#1236,#1000),#3682,.F.);
#3919=CLOSED_SHELL('',(#3683,#3684,#3685,#3686,#3687,#3688,#3689,#3690,
#3691,#3692,#3693,#3694,#3695,#3696,#3697,#3698,#3699,#3700,#3701,#3702,
#3703,#3704,#3705,#3706,#3707));
#3920=CLOSED_SHELL('',(#3708,#3709,#3710,#3711,#3712,#3713,#3714,#3715,
#3716));
#3921=CLOSED_SHELL('',(#3717,#3718,#3719,#3720));
#3922=CLOSED_SHELL('',(#3721,#3722,#3723,#3724,#3725,#3726,#3727));
#3923=CLOSED_SHELL('',(#3728,#3729,#3730,#3731));
#3924=CLOSED_SHELL('',(#3732,#3733,#3734,#3735));
#3925=CLOSED_SHELL('',(#3736,#3737,#3738,#3739));
#3926=CLOSED_SHELL('',(#3740,#3741,#3742,#3743));
#3927=CLOSED_SHELL('',(#3744,#3745,#3746,#3747,#3748,#3749,#3750,#3751));
#3928=CLOSED_SHELL('',(#3752,#3753,#3754,#3755,#3756,#3757,#3758,#3759,
#3760,#3761));
#3929=CLOSED_SHELL('',(#3762,#3763,#3764,#3765));
#3930=CLOSED_SHELL('',(#3766,#3767,#3768,#3769,#3770,#3771,#3772,#3773,
#3774,#3775,#3776));
#3931=CLOSED_SHELL('',(#3777,#3778,#3779,#3780,#3781,#3782,#3783,#3784,
#3785));
#3932=CLOSED_SHELL('',(#3786,#3787,#3788,#3789,#3790,#3791,#3792,#3793));
#3933=CLOSED_SHELL('',(#3794,#3795,#3796,#3797,#3798,#3799,#3800,#3801,
#3802,#3803,#3804,#3805,#3806,#3807,#3808));
#3934=CLOSED_SHELL('',(#3809,#3810,#3811,#3812));
#3935=CLOSED_SHELL('',(#3813,#3814,#3815,#3816,#3817,#3818,#3819,#3820));
#3936=CLOSED_SHELL('',(#3821,#3822,#3823,#3824,#3825,#3826,#3827,#3828));
#3937=CLOSED_SHELL('',(#3829));
#3938=CLOSED_SHELL('',(#3830));
#3939=CLOSED_SHELL('',(#3831));
#3940=CLOSED_SHELL('',(#3832));
#3941=CLOSED_SHELL('',(#3833));
#3942=CLOSED_SHELL('',(#3834));
#3943=CLOSED_SHELL('',(#3835));
#3944=CLOSED_SHELL('',(#3836));
#3945=CLOSED_SHELL('',(#3837,#3838,#3839,#3840,#3841,#3842,#3843,#3844,
#3845,#3846,#3847,#3848,#3849,#3850,#3851,#3852,#3853,#3854,#3855));
#3946=CLOSED_SHELL('',(#3856,#3857,#3858,#3859));
#3947=CLOSED_SHELL('',(#3860,#3861,#3862,#3863));
#3948=CLOSED_SHELL('',(#3864,#3865,#3866,#3867,#3868,#3869,#3870,#3871,
#3872,#3873));
#3949=CLOSED_SHELL('',(#3874,#3875,#3876,#3877,#3878,#3879,#3880,#3881));
#3950=CLOSED_SHELL('',(#3882,#3883,#3884,#3885,#3886,#3887,#3888,#3889));
#3951=CLOSED_SHELL('',(#3890,#3891,#3892,#3893,#3894,#3895,#3896,#3897,
#3898,#3899,#3900,#3901,#3902,#3903,#3904,#3905));
#3952=CLOSED_SHELL('',(#3906,#3907,#3908,#3909));
#3953=CLOSED_SHELL('',(#3910,#3911,#3912,#3913,#3914,#3915,#3916,#3917,
#3918));
#3954=DERIVED_UNIT_ELEMENT(#4002,1.);
#3955=DERIVED_UNIT_ELEMENT(#7611,-3.);
#3956=DERIVED_UNIT_ELEMENT(#4002,1.);
#3957=DERIVED_UNIT_ELEMENT(#7611,-3.);
#3958=DERIVED_UNIT_ELEMENT(#4002,1.);
#3959=DERIVED_UNIT_ELEMENT(#7611,-3.);
#3960=DERIVED_UNIT_ELEMENT(#4002,1.);
#3961=DERIVED_UNIT_ELEMENT(#7611,-3.);
#3962=DERIVED_UNIT_ELEMENT(#4002,1.);
#3963=DERIVED_UNIT_ELEMENT(#7611,-3.);
#3964=DERIVED_UNIT_ELEMENT(#4002,1.);
#3965=DERIVED_UNIT_ELEMENT(#7611,-3.);
#3966=DERIVED_UNIT_ELEMENT(#4002,1.);
#3967=DERIVED_UNIT_ELEMENT(#7611,-3.);
#3968=DERIVED_UNIT_ELEMENT(#4002,1.);
#3969=DERIVED_UNIT_ELEMENT(#7611,-3.);
#3970=DERIVED_UNIT_ELEMENT(#4002,1.);
#3971=DERIVED_UNIT_ELEMENT(#7611,-3.);
#3972=DERIVED_UNIT_ELEMENT(#4002,1.);
#3973=DERIVED_UNIT_ELEMENT(#7611,-3.);
#3974=DERIVED_UNIT_ELEMENT(#4002,1.);
#3975=DERIVED_UNIT_ELEMENT(#7611,-3.);
#3976=DERIVED_UNIT_ELEMENT(#4002,1.);
#3977=DERIVED_UNIT_ELEMENT(#7611,-3.);
#3978=DERIVED_UNIT_ELEMENT(#4002,1.);
#3979=DERIVED_UNIT_ELEMENT(#7611,-3.);
#3980=DERIVED_UNIT_ELEMENT(#4002,1.);
#3981=DERIVED_UNIT_ELEMENT(#7611,-3.);
#3982=DERIVED_UNIT_ELEMENT(#4002,1.);
#3983=DERIVED_UNIT_ELEMENT(#7611,-3.);
#3984=DERIVED_UNIT_ELEMENT(#4002,1.);
#3985=DERIVED_UNIT_ELEMENT(#7611,-3.);
#3986=DERIVED_UNIT_ELEMENT(#4002,1.);
#3987=DERIVED_UNIT_ELEMENT(#7611,-3.);
#3988=DERIVED_UNIT_ELEMENT(#4002,1.);
#3989=DERIVED_UNIT_ELEMENT(#7611,-3.);
#3990=DERIVED_UNIT_ELEMENT(#4002,1.);
#3991=DERIVED_UNIT_ELEMENT(#7611,-3.);
#3992=DERIVED_UNIT_ELEMENT(#4002,1.);
#3993=DERIVED_UNIT_ELEMENT(#7611,-3.);
#3994=DERIVED_UNIT_ELEMENT(#4002,1.);
#3995=DERIVED_UNIT_ELEMENT(#7611,-3.);
#3996=DERIVED_UNIT_ELEMENT(#4002,1.);
#3997=DERIVED_UNIT_ELEMENT(#7611,-3.);
#3998=DERIVED_UNIT_ELEMENT(#4002,1.);
#3999=DERIVED_UNIT_ELEMENT(#7611,-3.);
#4000=DERIVED_UNIT_ELEMENT(#4002,1.);
#4001=DERIVED_UNIT_ELEMENT(#7611,-3.);
#4002=(
MASS_UNIT()
NAMED_UNIT(*)
SI_UNIT(.KILO.,.GRAM.)
);
#4003=DERIVED_UNIT((#3954,#3955));
#4004=DERIVED_UNIT((#3956,#3957));
#4005=DERIVED_UNIT((#3958,#3959));
#4006=DERIVED_UNIT((#3960,#3961));
#4007=DERIVED_UNIT((#3962,#3963));
#4008=DERIVED_UNIT((#3964,#3965));
#4009=DERIVED_UNIT((#3966,#3967));
#4010=DERIVED_UNIT((#3968,#3969));
#4011=DERIVED_UNIT((#3970,#3971));
#4012=DERIVED_UNIT((#3972,#3973));
#4013=DERIVED_UNIT((#3974,#3975));
#4014=DERIVED_UNIT((#3976,#3977));
#4015=DERIVED_UNIT((#3978,#3979));
#4016=DERIVED_UNIT((#3980,#3981));
#4017=DERIVED_UNIT((#3982,#3983));
#4018=DERIVED_UNIT((#3984,#3985));
#4019=DERIVED_UNIT((#3986,#3987));
#4020=DERIVED_UNIT((#3988,#3989));
#4021=DERIVED_UNIT((#3990,#3991));
#4022=DERIVED_UNIT((#3992,#3993));
#4023=DERIVED_UNIT((#3994,#3995));
#4024=DERIVED_UNIT((#3996,#3997));
#4025=DERIVED_UNIT((#3998,#3999));
#4026=DERIVED_UNIT((#4000,#4001));
#4027=MEASURE_REPRESENTATION_ITEM('density measure',
POSITIVE_RATIO_MEASURE(7850.),#4003);
#4028=MEASURE_REPRESENTATION_ITEM('density measure',
POSITIVE_RATIO_MEASURE(7850.),#4004);
#4029=MEASURE_REPRESENTATION_ITEM('density measure',
POSITIVE_RATIO_MEASURE(7850.),#4005);
#4030=MEASURE_REPRESENTATION_ITEM('density measure',
POSITIVE_RATIO_MEASURE(7850.),#4006);
#4031=MEASURE_REPRESENTATION_ITEM('density measure',
POSITIVE_RATIO_MEASURE(7850.),#4007);
#4032=MEASURE_REPRESENTATION_ITEM('density measure',
POSITIVE_RATIO_MEASURE(7850.),#4008);
#4033=MEASURE_REPRESENTATION_ITEM('density measure',
POSITIVE_RATIO_MEASURE(7850.),#4009);
#4034=MEASURE_REPRESENTATION_ITEM('density measure',
POSITIVE_RATIO_MEASURE(7850.),#4010);
#4035=MEASURE_REPRESENTATION_ITEM('density measure',
POSITIVE_RATIO_MEASURE(7850.),#4011);
#4036=MEASURE_REPRESENTATION_ITEM('density measure',
POSITIVE_RATIO_MEASURE(7850.),#4012);
#4037=MEASURE_REPRESENTATION_ITEM('density measure',
POSITIVE_RATIO_MEASURE(7850.),#4013);
#4038=MEASURE_REPRESENTATION_ITEM('density measure',
POSITIVE_RATIO_MEASURE(7850.),#4014);
#4039=MEASURE_REPRESENTATION_ITEM('density measure',
POSITIVE_RATIO_MEASURE(7850.),#4015);
#4040=MEASURE_REPRESENTATION_ITEM('density measure',
POSITIVE_RATIO_MEASURE(7850.),#4016);
#4041=MEASURE_REPRESENTATION_ITEM('density measure',
POSITIVE_RATIO_MEASURE(7850.),#4017);
#4042=MEASURE_REPRESENTATION_ITEM('density measure',
POSITIVE_RATIO_MEASURE(7850.),#4018);
#4043=MEASURE_REPRESENTATION_ITEM('density measure',
POSITIVE_RATIO_MEASURE(7850.),#4019);
#4044=MEASURE_REPRESENTATION_ITEM('density measure',
POSITIVE_RATIO_MEASURE(7850.),#4020);
#4045=MEASURE_REPRESENTATION_ITEM('density measure',
POSITIVE_RATIO_MEASURE(7850.),#4021);
#4046=MEASURE_REPRESENTATION_ITEM('density measure',
POSITIVE_RATIO_MEASURE(7850.),#4022);
#4047=MEASURE_REPRESENTATION_ITEM('density measure',
POSITIVE_RATIO_MEASURE(7850.),#4023);
#4048=MEASURE_REPRESENTATION_ITEM('density measure',
POSITIVE_RATIO_MEASURE(7850.),#4024);
#4049=MEASURE_REPRESENTATION_ITEM('density measure',
POSITIVE_RATIO_MEASURE(7850.),#4025);
#4050=MEASURE_REPRESENTATION_ITEM('density measure',
POSITIVE_RATIO_MEASURE(7850.),#4026);
#4051=PROPERTY_DEFINITION_REPRESENTATION(#4171,#4099);
#4052=PROPERTY_DEFINITION_REPRESENTATION(#4172,#4100);
#4053=PROPERTY_DEFINITION_REPRESENTATION(#4173,#4101);
#4054=PROPERTY_DEFINITION_REPRESENTATION(#4174,#4102);
#4055=PROPERTY_DEFINITION_REPRESENTATION(#4175,#4103);
#4056=PROPERTY_DEFINITION_REPRESENTATION(#4176,#4104);
#4057=PROPERTY_DEFINITION_REPRESENTATION(#4177,#4105);
#4058=PROPERTY_DEFINITION_REPRESENTATION(#4178,#4106);
#4059=PROPERTY_DEFINITION_REPRESENTATION(#4179,#4107);
#4060=PROPERTY_DEFINITION_REPRESENTATION(#4180,#4108);
#4061=PROPERTY_DEFINITION_REPRESENTATION(#4181,#4109);
#4062=PROPERTY_DEFINITION_REPRESENTATION(#4182,#4110);
#4063=PROPERTY_DEFINITION_REPRESENTATION(#4183,#4111);
#4064=PROPERTY_DEFINITION_REPRESENTATION(#4184,#4112);
#4065=PROPERTY_DEFINITION_REPRESENTATION(#4185,#4113);
#4066=PROPERTY_DEFINITION_REPRESENTATION(#4186,#4114);
#4067=PROPERTY_DEFINITION_REPRESENTATION(#4187,#4115);
#4068=PROPERTY_DEFINITION_REPRESENTATION(#4188,#4116);
#4069=PROPERTY_DEFINITION_REPRESENTATION(#4189,#4117);
#4070=PROPERTY_DEFINITION_REPRESENTATION(#4190,#4118);
#4071=PROPERTY_DEFINITION_REPRESENTATION(#4191,#4119);
#4072=PROPERTY_DEFINITION_REPRESENTATION(#4192,#4120);
#4073=PROPERTY_DEFINITION_REPRESENTATION(#4193,#4121);
#4074=PROPERTY_DEFINITION_REPRESENTATION(#4194,#4122);
#4075=PROPERTY_DEFINITION_REPRESENTATION(#4195,#4123);
#4076=PROPERTY_DEFINITION_REPRESENTATION(#4196,#4124);
#4077=PROPERTY_DEFINITION_REPRESENTATION(#4197,#4125);
#4078=PROPERTY_DEFINITION_REPRESENTATION(#4198,#4126);
#4079=PROPERTY_DEFINITION_REPRESENTATION(#4199,#4127);
#4080=PROPERTY_DEFINITION_REPRESENTATION(#4200,#4128);
#4081=PROPERTY_DEFINITION_REPRESENTATION(#4201,#4129);
#4082=PROPERTY_DEFINITION_REPRESENTATION(#4202,#4130);
#4083=PROPERTY_DEFINITION_REPRESENTATION(#4203,#4131);
#4084=PROPERTY_DEFINITION_REPRESENTATION(#4204,#4132);
#4085=PROPERTY_DEFINITION_REPRESENTATION(#4205,#4133);
#4086=PROPERTY_DEFINITION_REPRESENTATION(#4206,#4134);
#4087=PROPERTY_DEFINITION_REPRESENTATION(#4207,#4135);
#4088=PROPERTY_DEFINITION_REPRESENTATION(#4208,#4136);
#4089=PROPERTY_DEFINITION_REPRESENTATION(#4209,#4137);
#4090=PROPERTY_DEFINITION_REPRESENTATION(#4210,#4138);
#4091=PROPERTY_DEFINITION_REPRESENTATION(#4211,#4139);
#4092=PROPERTY_DEFINITION_REPRESENTATION(#4212,#4140);
#4093=PROPERTY_DEFINITION_REPRESENTATION(#4213,#4141);
#4094=PROPERTY_DEFINITION_REPRESENTATION(#4214,#4142);
#4095=PROPERTY_DEFINITION_REPRESENTATION(#4215,#4143);
#4096=PROPERTY_DEFINITION_REPRESENTATION(#4216,#4144);
#4097=PROPERTY_DEFINITION_REPRESENTATION(#4217,#4145);
#4098=PROPERTY_DEFINITION_REPRESENTATION(#4218,#4146);
#4099=REPRESENTATION('material name',(#4147),#7582);
#4100=REPRESENTATION('density',(#4027),#7582);
#4101=REPRESENTATION('material name',(#4148),#7583);
#4102=REPRESENTATION('density',(#4028),#7583);
#4103=REPRESENTATION('material name',(#4149),#7584);
#4104=REPRESENTATION('density',(#4029),#7584);
#4105=REPRESENTATION('material name',(#4150),#7585);
#4106=REPRESENTATION('density',(#4030),#7585);
#4107=REPRESENTATION('material name',(#4151),#7586);
#4108=REPRESENTATION('density',(#4031),#7586);
#4109=REPRESENTATION('material name',(#4152),#7587);
#4110=REPRESENTATION('density',(#4032),#7587);
#4111=REPRESENTATION('material name',(#4153),#7588);
#4112=REPRESENTATION('density',(#4033),#7588);
#4113=REPRESENTATION('material name',(#4154),#7589);
#4114=REPRESENTATION('density',(#4034),#7589);
#4115=REPRESENTATION('material name',(#4155),#7590);
#4116=REPRESENTATION('density',(#4035),#7590);
#4117=REPRESENTATION('material name',(#4156),#7591);
#4118=REPRESENTATION('density',(#4036),#7591);
#4119=REPRESENTATION('material name',(#4157),#7592);
#4120=REPRESENTATION('density',(#4037),#7592);
#4121=REPRESENTATION('material name',(#4158),#7593);
#4122=REPRESENTATION('density',(#4038),#7593);
#4123=REPRESENTATION('material name',(#4159),#7595);
#4124=REPRESENTATION('density',(#4039),#7595);
#4125=REPRESENTATION('material name',(#4160),#7596);
#4126=REPRESENTATION('density',(#4040),#7596);
#4127=REPRESENTATION('material name',(#4161),#7598);
#4128=REPRESENTATION('density',(#4041),#7598);
#4129=REPRESENTATION('material name',(#4162),#7599);
#4130=REPRESENTATION('density',(#4042),#7599);
#4131=REPRESENTATION('material name',(#4163),#7600);
#4132=REPRESENTATION('density',(#4043),#7600);
#4133=REPRESENTATION('material name',(#4164),#7601);
#4134=REPRESENTATION('density',(#4044),#7601);
#4135=REPRESENTATION('material name',(#4165),#7602);
#4136=REPRESENTATION('density',(#4045),#7602);
#4137=REPRESENTATION('material name',(#4166),#7603);
#4138=REPRESENTATION('density',(#4046),#7603);
#4139=REPRESENTATION('material name',(#4167),#7604);
#4140=REPRESENTATION('density',(#4047),#7604);
#4141=REPRESENTATION('material name',(#4168),#7606);
#4142=REPRESENTATION('density',(#4048),#7606);
#4143=REPRESENTATION('material name',(#4169),#7607);
#4144=REPRESENTATION('density',(#4049),#7607);
#4145=REPRESENTATION('material name',(#4170),#7608);
#4146=REPRESENTATION('density',(#4050),#7608);
#4147=DESCRIPTIVE_REPRESENTATION_ITEM('Steel','Steel');
#4148=DESCRIPTIVE_REPRESENTATION_ITEM('Steel','Steel');
#4149=DESCRIPTIVE_REPRESENTATION_ITEM('Steel','Steel');
#4150=DESCRIPTIVE_REPRESENTATION_ITEM('Steel','Steel');
#4151=DESCRIPTIVE_REPRESENTATION_ITEM('Steel','Steel');
#4152=DESCRIPTIVE_REPRESENTATION_ITEM('Steel','Steel');
#4153=DESCRIPTIVE_REPRESENTATION_ITEM('Steel','Steel');
#4154=DESCRIPTIVE_REPRESENTATION_ITEM('Steel','Steel');
#4155=DESCRIPTIVE_REPRESENTATION_ITEM('Steel','Steel');
#4156=DESCRIPTIVE_REPRESENTATION_ITEM('Steel','Steel');
#4157=DESCRIPTIVE_REPRESENTATION_ITEM('Steel','Steel');
#4158=DESCRIPTIVE_REPRESENTATION_ITEM('Steel','Steel');
#4159=DESCRIPTIVE_REPRESENTATION_ITEM('Steel','Steel');
#4160=DESCRIPTIVE_REPRESENTATION_ITEM('Steel','Steel');
#4161=DESCRIPTIVE_REPRESENTATION_ITEM('Steel','Steel');
#4162=DESCRIPTIVE_REPRESENTATION_ITEM('Steel','Steel');
#4163=DESCRIPTIVE_REPRESENTATION_ITEM('Steel','Steel');
#4164=DESCRIPTIVE_REPRESENTATION_ITEM('Steel','Steel');
#4165=DESCRIPTIVE_REPRESENTATION_ITEM('Steel','Steel');
#4166=DESCRIPTIVE_REPRESENTATION_ITEM('Steel','Steel');
#4167=DESCRIPTIVE_REPRESENTATION_ITEM('Steel','Steel');
#4168=DESCRIPTIVE_REPRESENTATION_ITEM('Steel','Steel');
#4169=DESCRIPTIVE_REPRESENTATION_ITEM('Steel','Steel');
#4170=DESCRIPTIVE_REPRESENTATION_ITEM('Steel','Steel');
#4171=PROPERTY_DEFINITION('material property','material name',#7752);
#4172=PROPERTY_DEFINITION('material property','density of part',#7752);
#4173=PROPERTY_DEFINITION('material property','material name',#7753);
#4174=PROPERTY_DEFINITION('material property','density of part',#7753);
#4175=PROPERTY_DEFINITION('material property','material name',#7754);
#4176=PROPERTY_DEFINITION('material property','density of part',#7754);
#4177=PROPERTY_DEFINITION('material property','material name',#7755);
#4178=PROPERTY_DEFINITION('material property','density of part',#7755);
#4179=PROPERTY_DEFINITION('material property','material name',#7756);
#4180=PROPERTY_DEFINITION('material property','density of part',#7756);
#4181=PROPERTY_DEFINITION('material property','material name',#7757);
#4182=PROPERTY_DEFINITION('material property','density of part',#7757);
#4183=PROPERTY_DEFINITION('material property','material name',#7758);
#4184=PROPERTY_DEFINITION('material property','density of part',#7758);
#4185=PROPERTY_DEFINITION('material property','material name',#7759);
#4186=PROPERTY_DEFINITION('material property','density of part',#7759);
#4187=PROPERTY_DEFINITION('material property','material name',#7760);
#4188=PROPERTY_DEFINITION('material property','density of part',#7760);
#4189=PROPERTY_DEFINITION('material property','material name',#7761);
#4190=PROPERTY_DEFINITION('material property','density of part',#7761);
#4191=PROPERTY_DEFINITION('material property','material name',#7762);
#4192=PROPERTY_DEFINITION('material property','density of part',#7762);
#4193=PROPERTY_DEFINITION('material property','material name',#7763);
#4194=PROPERTY_DEFINITION('material property','density of part',#7763);
#4195=PROPERTY_DEFINITION('material property','material name',#7765);
#4196=PROPERTY_DEFINITION('material property','density of part',#7765);
#4197=PROPERTY_DEFINITION('material property','material name',#7766);
#4198=PROPERTY_DEFINITION('material property','density of part',#7766);
#4199=PROPERTY_DEFINITION('material property','material name',#7768);
#4200=PROPERTY_DEFINITION('material property','density of part',#7768);
#4201=PROPERTY_DEFINITION('material property','material name',#7769);
#4202=PROPERTY_DEFINITION('material property','density of part',#7769);
#4203=PROPERTY_DEFINITION('material property','material name',#7770);
#4204=PROPERTY_DEFINITION('material property','density of part',#7770);
#4205=PROPERTY_DEFINITION('material property','material name',#7771);
#4206=PROPERTY_DEFINITION('material property','density of part',#7771);
#4207=PROPERTY_DEFINITION('material property','material name',#7772);
#4208=PROPERTY_DEFINITION('material property','density of part',#7772);
#4209=PROPERTY_DEFINITION('material property','material name',#7773);
#4210=PROPERTY_DEFINITION('material property','density of part',#7773);
#4211=PROPERTY_DEFINITION('material property','material name',#7774);
#4212=PROPERTY_DEFINITION('material property','density of part',#7774);
#4213=PROPERTY_DEFINITION('material property','material name',#7776);
#4214=PROPERTY_DEFINITION('material property','density of part',#7776);
#4215=PROPERTY_DEFINITION('material property','material name',#7777);
#4216=PROPERTY_DEFINITION('material property','density of part',#7777);
#4217=PROPERTY_DEFINITION('material property','material name',#7778);
#4218=PROPERTY_DEFINITION('material property','density of part',#7778);
#4219=AXIS2_PLACEMENT_3D('',#6063,#4757,#4758);
#4220=AXIS2_PLACEMENT_3D('',#6064,#4759,#4760);
#4221=AXIS2_PLACEMENT_3D('',#6065,#4761,#4762);
#4222=AXIS2_PLACEMENT_3D('',#6066,#4763,#4764);
#4223=AXIS2_PLACEMENT_3D('',#6069,#4765,#4766);
#4224=AXIS2_PLACEMENT_3D('',#6071,#4767,#4768);
#4225=AXIS2_PLACEMENT_3D('',#6073,#4769,#4770);
#4226=AXIS2_PLACEMENT_3D('',#6075,#4771,#4772);
#4227=AXIS2_PLACEMENT_3D('',#6077,#4773,#4774);
#4228=AXIS2_PLACEMENT_3D('',#6079,#4775,#4776);
#4229=AXIS2_PLACEMENT_3D('',#6081,#4777,#4778);
#4230=AXIS2_PLACEMENT_3D('',#6082,#4779,#4780);
#4231=AXIS2_PLACEMENT_3D('',#6084,#4781,#4782);
#4232=AXIS2_PLACEMENT_3D('',#6085,#4783,#4784);
#4233=AXIS2_PLACEMENT_3D('',#6090,#4787,#4788);
#4234=AXIS2_PLACEMENT_3D('',#6091,#4789,#4790);
#4235=AXIS2_PLACEMENT_3D('',#6095,#4792,#4793);
#4236=AXIS2_PLACEMENT_3D('',#6097,#4795,#4796);
#4237=AXIS2_PLACEMENT_3D('',#6102,#4799,#4800);
#4238=AXIS2_PLACEMENT_3D('',#6103,#4801,#4802);
#4239=AXIS2_PLACEMENT_3D('',#6106,#4804,#4805);
#4240=AXIS2_PLACEMENT_3D('',#6107,#4806,#4807);
#4241=AXIS2_PLACEMENT_3D('',#6111,#4809,#4810);
#4242=AXIS2_PLACEMENT_3D('',#6113,#4812,#4813);
#4243=AXIS2_PLACEMENT_3D('',#6115,#4814,#4815);
#4244=AXIS2_PLACEMENT_3D('',#6118,#4817,#4818);
#4245=AXIS2_PLACEMENT_3D('',#6119,#4819,#4820);
#4246=AXIS2_PLACEMENT_3D('',#6120,#4821,#4822);
#4247=AXIS2_PLACEMENT_3D('',#6122,#4823,#4824);
#4248=AXIS2_PLACEMENT_3D('',#6125,#4826,#4827);
#4249=AXIS2_PLACEMENT_3D('',#6126,#4828,#4829);
#4250=AXIS2_PLACEMENT_3D('',#6127,#4830,#4831);
#4251=AXIS2_PLACEMENT_3D('',#6129,#4832,#4833);
#4252=AXIS2_PLACEMENT_3D('',#6132,#4835,#4836);
#4253=AXIS2_PLACEMENT_3D('',#6133,#4837,#4838);
#4254=AXIS2_PLACEMENT_3D('',#6134,#4839,#4840);
#4255=AXIS2_PLACEMENT_3D('',#6136,#4841,#4842);
#4256=AXIS2_PLACEMENT_3D('',#6137,#4843,#4844);
#4257=AXIS2_PLACEMENT_3D('',#6139,#4845,#4846);
#4258=AXIS2_PLACEMENT_3D('',#6142,#4848,#4849);
#4259=AXIS2_PLACEMENT_3D('',#6143,#4850,#4851);
#4260=AXIS2_PLACEMENT_3D('',#6144,#4852,#4853);
#4261=AXIS2_PLACEMENT_3D('',#6146,#4854,#4855);
#4262=AXIS2_PLACEMENT_3D('',#6149,#4857,#4858);
#4263=AXIS2_PLACEMENT_3D('',#6150,#4859,#4860);
#4264=AXIS2_PLACEMENT_3D('',#6152,#4861,#4862);
#4265=AXIS2_PLACEMENT_3D('',#6155,#4864,#4865);
#4266=AXIS2_PLACEMENT_3D('',#6156,#4866,#4867);
#4267=AXIS2_PLACEMENT_3D('',#6158,#4868,#4869);
#4268=AXIS2_PLACEMENT_3D('',#6161,#4871,#4872);
#4269=AXIS2_PLACEMENT_3D('',#6162,#4873,#4874);
#4270=AXIS2_PLACEMENT_3D('',#6164,#4875,#4876);
#4271=AXIS2_PLACEMENT_3D('',#6166,#4878,#4879);
#4272=AXIS2_PLACEMENT_3D('',#6175,#4884,#4885);
#4273=AXIS2_PLACEMENT_3D('',#6181,#4889,#4890);
#4274=AXIS2_PLACEMENT_3D('',#6187,#4894,#4895);
#4275=AXIS2_PLACEMENT_3D('',#6193,#4899,#4900);
#4276=AXIS2_PLACEMENT_3D('',#6199,#4904,#4905);
#4277=AXIS2_PLACEMENT_3D('',#6205,#4909,#4910);
#4278=AXIS2_PLACEMENT_3D('',#6211,#4914,#4915);
#4279=AXIS2_PLACEMENT_3D('',#6214,#4918,#4919);
#4280=AXIS2_PLACEMENT_3D('',#6215,#4920,#4921);
#4281=AXIS2_PLACEMENT_3D('',#6216,#4922,#4923);
#4282=AXIS2_PLACEMENT_3D('',#6217,#4924,#4925);
#4283=AXIS2_PLACEMENT_3D('',#6219,#4926,#4927);
#4284=AXIS2_PLACEMENT_3D('',#6222,#4929,#4930);
#4285=AXIS2_PLACEMENT_3D('',#6223,#4931,#4932);
#4286=AXIS2_PLACEMENT_3D('',#6225,#4933,#4934);
#4287=AXIS2_PLACEMENT_3D('',#6228,#4936,#4937);
#4288=AXIS2_PLACEMENT_3D('',#6229,#4938,#4939);
#4289=AXIS2_PLACEMENT_3D('',#6231,#4940,#4941);
#4290=AXIS2_PLACEMENT_3D('',#6234,#4943,#4944);
#4291=AXIS2_PLACEMENT_3D('',#6235,#4945,#4946);
#4292=AXIS2_PLACEMENT_3D('',#6244,#4951,#4952);
#4293=AXIS2_PLACEMENT_3D('',#6250,#4956,#4957);
#4294=AXIS2_PLACEMENT_3D('',#6256,#4961,#4962);
#4295=AXIS2_PLACEMENT_3D('',#6259,#4965,#4966);
#4296=AXIS2_PLACEMENT_3D('',#6260,#4967,#4968);
#4297=AXIS2_PLACEMENT_3D('',#6261,#4969,#4970);
#4298=AXIS2_PLACEMENT_3D('',#6262,#4971,#4972);
#4299=AXIS2_PLACEMENT_3D('',#6264,#4973,#4974);
#4300=AXIS2_PLACEMENT_3D('',#6267,#4976,#4977);
#4301=AXIS2_PLACEMENT_3D('',#6268,#4978,#4979);
#4302=AXIS2_PLACEMENT_3D('',#6270,#4980,#4981);
#4303=AXIS2_PLACEMENT_3D('',#6273,#4983,#4984);
#4304=AXIS2_PLACEMENT_3D('',#6274,#4985,#4986);
#4305=AXIS2_PLACEMENT_3D('',#6275,#4987,#4988);
#4306=AXIS2_PLACEMENT_3D('',#6276,#4989,#4990);
#4307=AXIS2_PLACEMENT_3D('',#6277,#4991,#4992);
#4308=AXIS2_PLACEMENT_3D('',#6279,#4993,#4994);
#4309=AXIS2_PLACEMENT_3D('',#6282,#4996,#4997);
#4310=AXIS2_PLACEMENT_3D('',#6283,#4998,#4999);
#4311=AXIS2_PLACEMENT_3D('',#6284,#5000,#5001);
#4312=AXIS2_PLACEMENT_3D('',#6286,#5002,#5003);
#4313=AXIS2_PLACEMENT_3D('',#6288,#5004,#5005);
#4314=AXIS2_PLACEMENT_3D('',#6289,#5006,#5007);
#4315=AXIS2_PLACEMENT_3D('',#6292,#5009,#5010);
#4316=AXIS2_PLACEMENT_3D('',#6293,#5011,#5012);
#4317=AXIS2_PLACEMENT_3D('',#6294,#5013,#5014);
#4318=AXIS2_PLACEMENT_3D('',#6296,#5015,#5016);
#4319=AXIS2_PLACEMENT_3D('',#6298,#5018,#5019);
#4320=AXIS2_PLACEMENT_3D('',#6299,#5020,#5021);
#4321=AXIS2_PLACEMENT_3D('',#6300,#5022,#5023);
#4322=AXIS2_PLACEMENT_3D('',#6302,#5024,#5025);
#4323=AXIS2_PLACEMENT_3D('',#6305,#5027,#5028);
#4324=AXIS2_PLACEMENT_3D('',#6306,#5029,#5030);
#4325=AXIS2_PLACEMENT_3D('',#6308,#5031,#5032);
#4326=AXIS2_PLACEMENT_3D('',#6311,#5034,#5035);
#4327=AXIS2_PLACEMENT_3D('',#6312,#5036,#5037);
#4328=AXIS2_PLACEMENT_3D('',#6313,#5038,#5039);
#4329=AXIS2_PLACEMENT_3D('',#6314,#5040,#5041);
#4330=AXIS2_PLACEMENT_3D('',#6315,#5042,#5043);
#4331=AXIS2_PLACEMENT_3D('',#6317,#5044,#5045);
#4332=AXIS2_PLACEMENT_3D('',#6320,#5047,#5048);
#4333=AXIS2_PLACEMENT_3D('',#6321,#5049,#5050);
#4334=AXIS2_PLACEMENT_3D('',#6323,#5051,#5052);
#4335=AXIS2_PLACEMENT_3D('',#6326,#5054,#5055);
#4336=AXIS2_PLACEMENT_3D('',#6327,#5056,#5057);
#4337=AXIS2_PLACEMENT_3D('',#6328,#5058,#5059);
#4338=AXIS2_PLACEMENT_3D('',#6329,#5060,#5061);
#4339=AXIS2_PLACEMENT_3D('',#6330,#5062,#5063);
#4340=AXIS2_PLACEMENT_3D('',#6332,#5064,#5065);
#4341=AXIS2_PLACEMENT_3D('',#6335,#5067,#5068);
#4342=AXIS2_PLACEMENT_3D('',#6336,#5069,#5070);
#4343=AXIS2_PLACEMENT_3D('',#6338,#5071,#5072);
#4344=AXIS2_PLACEMENT_3D('',#6341,#5074,#5075);
#4345=AXIS2_PLACEMENT_3D('',#6342,#5076,#5077);
#4346=AXIS2_PLACEMENT_3D('',#6343,#5078,#5079);
#4347=AXIS2_PLACEMENT_3D('',#6344,#5080,#5081);
#4348=AXIS2_PLACEMENT_3D('',#6345,#5082,#5083);
#4349=AXIS2_PLACEMENT_3D('',#6347,#5084,#5085);
#4350=AXIS2_PLACEMENT_3D('',#6350,#5087,#5088);
#4351=AXIS2_PLACEMENT_3D('',#6351,#5089,#5090);
#4352=AXIS2_PLACEMENT_3D('',#6353,#5091,#5092);
#4353=AXIS2_PLACEMENT_3D('',#6356,#5094,#5095);
#4354=AXIS2_PLACEMENT_3D('',#6357,#5096,#5097);
#4355=AXIS2_PLACEMENT_3D('',#6358,#5098,#5099);
#4356=AXIS2_PLACEMENT_3D('',#6359,#5100,#5101);
#4357=AXIS2_PLACEMENT_3D('',#6360,#5102,#5103);
#4358=AXIS2_PLACEMENT_3D('',#6369,#5108,#5109);
#4359=AXIS2_PLACEMENT_3D('',#6375,#5113,#5114);
#4360=AXIS2_PLACEMENT_3D('',#6381,#5118,#5119);
#4361=AXIS2_PLACEMENT_3D('',#6387,#5123,#5124);
#4362=AXIS2_PLACEMENT_3D('',#6393,#5128,#5129);
#4363=AXIS2_PLACEMENT_3D('',#6396,#5132,#5133);
#4364=AXIS2_PLACEMENT_3D('',#6397,#5134,#5135);
#4365=AXIS2_PLACEMENT_3D('',#6398,#5136,#5137);
#4366=AXIS2_PLACEMENT_3D('',#6400,#5138,#5139);
#4367=AXIS2_PLACEMENT_3D('',#6402,#5140,#5141);
#4368=AXIS2_PLACEMENT_3D('',#6403,#5142,#5143);
#4369=AXIS2_PLACEMENT_3D('',#6406,#5145,#5146);
#4370=AXIS2_PLACEMENT_3D('',#6407,#5147,#5148);
#4371=AXIS2_PLACEMENT_3D('',#6408,#5149,#5150);
#4372=AXIS2_PLACEMENT_3D('',#6410,#5151,#5152);
#4373=AXIS2_PLACEMENT_3D('',#6411,#5153,#5154);
#4374=AXIS2_PLACEMENT_3D('',#6413,#5155,#5156);
#4375=AXIS2_PLACEMENT_3D('',#6415,#5158,#5159);
#4376=AXIS2_PLACEMENT_3D('',#6417,#5160,#5161);
#4377=AXIS2_PLACEMENT_3D('',#6419,#5163,#5164);
#4378=AXIS2_PLACEMENT_3D('',#6421,#5165,#5166);
#4379=AXIS2_PLACEMENT_3D('',#6423,#5168,#5169);
#4380=AXIS2_PLACEMENT_3D('',#6425,#5170,#5171);
#4381=AXIS2_PLACEMENT_3D('',#6426,#5172,#5173);
#4382=AXIS2_PLACEMENT_3D('',#6428,#5174,#5175);
#4383=AXIS2_PLACEMENT_3D('',#6430,#5177,#5178);
#4384=AXIS2_PLACEMENT_3D('',#6432,#5180,#5181);
#4385=AXIS2_PLACEMENT_3D('',#6433,#5182,#5183);
#4386=AXIS2_PLACEMENT_3D('',#6435,#5184,#5185);
#4387=AXIS2_PLACEMENT_3D('',#6438,#5187,#5188);
#4388=AXIS2_PLACEMENT_3D('',#6439,#5189,#5190);
#4389=AXIS2_PLACEMENT_3D('',#6441,#5191,#5192);
#4390=AXIS2_PLACEMENT_3D('',#6444,#5194,#5195);
#4391=AXIS2_PLACEMENT_3D('',#6445,#5196,#5197);
#4392=AXIS2_PLACEMENT_3D('',#6446,#5198,#5199);
#4393=AXIS2_PLACEMENT_3D('',#6447,#5200,#5201);
#4394=AXIS2_PLACEMENT_3D('',#6448,#5202,#5203);
#4395=AXIS2_PLACEMENT_3D('',#6460,#5205,#5206);
#4396=AXIS2_PLACEMENT_3D('',#6476,#5207,#5208);
#4397=AXIS2_PLACEMENT_3D('',#6478,#5209,#5210);
#4398=AXIS2_PLACEMENT_3D('',#6504,#5212,#5213);
#4399=AXIS2_PLACEMENT_3D('',#6507,#5216,#5217);
#4400=AXIS2_PLACEMENT_3D('',#6509,#5219,#5220);
#4401=AXIS2_PLACEMENT_3D('',#6511,#5222,#5223);
#4402=AXIS2_PLACEMENT_3D('',#6513,#5224,#5225);
#4403=AXIS2_PLACEMENT_3D('',#6516,#5227,#5228);
#4404=AXIS2_PLACEMENT_3D('',#6517,#5229,#5230);
#4405=AXIS2_PLACEMENT_3D('',#6519,#5232,#5233);
#4406=AXIS2_PLACEMENT_3D('',#6521,#5235,#5236);
#4407=AXIS2_PLACEMENT_3D('',#6522,#5237,#5238);
#4408=AXIS2_PLACEMENT_3D('',#6523,#5239,#5240);
#4409=AXIS2_PLACEMENT_3D('',#6524,#5241,#5242);
#4410=AXIS2_PLACEMENT_3D('',#6525,#5243,#5244);
#4411=AXIS2_PLACEMENT_3D('',#6527,#5245,#5246);
#4412=AXIS2_PLACEMENT_3D('',#6528,#5247,#5248);
#4413=AXIS2_PLACEMENT_3D('',#6530,#5249,#5250);
#4414=AXIS2_PLACEMENT_3D('',#6532,#5252,#5253);
#4415=AXIS2_PLACEMENT_3D('',#6534,#5254,#5255);
#4416=AXIS2_PLACEMENT_3D('',#6536,#5257,#5258);
#4417=AXIS2_PLACEMENT_3D('',#6538,#5259,#5260);
#4418=AXIS2_PLACEMENT_3D('',#6540,#5262,#5263);
#4419=AXIS2_PLACEMENT_3D('',#6542,#5264,#5265);
#4420=AXIS2_PLACEMENT_3D('',#6543,#5266,#5267);
#4421=AXIS2_PLACEMENT_3D('',#6545,#5268,#5269);
#4422=AXIS2_PLACEMENT_3D('',#6547,#5271,#5272);
#4423=AXIS2_PLACEMENT_3D('',#6549,#5273,#5274);
#4424=AXIS2_PLACEMENT_3D('',#6551,#5276,#5277);
#4425=AXIS2_PLACEMENT_3D('',#6553,#5278,#5279);
#4426=AXIS2_PLACEMENT_3D('',#6555,#5281,#5282);
#4427=AXIS2_PLACEMENT_3D('',#6556,#5283,#5284);
#4428=AXIS2_PLACEMENT_3D('',#6565,#5289,#5290);
#4429=AXIS2_PLACEMENT_3D('',#6571,#5294,#5295);
#4430=AXIS2_PLACEMENT_3D('',#6577,#5299,#5300);
#4431=AXIS2_PLACEMENT_3D('',#6583,#5304,#5305);
#4432=AXIS2_PLACEMENT_3D('',#6589,#5309,#5310);
#4433=AXIS2_PLACEMENT_3D('',#6592,#5313,#5314);
#4434=AXIS2_PLACEMENT_3D('',#6593,#5315,#5316);
#4435=AXIS2_PLACEMENT_3D('',#6594,#5317,#5318);
#4436=AXIS2_PLACEMENT_3D('',#6595,#5319,#5320);
#4437=AXIS2_PLACEMENT_3D('',#6596,#5321,#5322);
#4438=AXIS2_PLACEMENT_3D('',#6597,#5323,#5324);
#4439=AXIS2_PLACEMENT_3D('',#6598,#5325,#5326);
#4440=AXIS2_PLACEMENT_3D('',#6599,#5327,#5328);
#4441=AXIS2_PLACEMENT_3D('',#6600,#5329,#5330);
#4442=AXIS2_PLACEMENT_3D('',#6601,#5331,#5332);
#4443=AXIS2_PLACEMENT_3D('',#6602,#5333,#5334);
#4444=AXIS2_PLACEMENT_3D('',#6603,#5335,#5336);
#4445=AXIS2_PLACEMENT_3D('',#6604,#5337,#5338);
#4446=AXIS2_PLACEMENT_3D('',#6605,#5339,#5340);
#4447=AXIS2_PLACEMENT_3D('',#6606,#5341,#5342);
#4448=AXIS2_PLACEMENT_3D('',#6607,#5343,#5344);
#4449=AXIS2_PLACEMENT_3D('',#6608,#5345,#5346);
#4450=AXIS2_PLACEMENT_3D('',#6609,#5347,#5348);
#4451=AXIS2_PLACEMENT_3D('',#6610,#5349,#5350);
#4452=AXIS2_PLACEMENT_3D('',#6611,#5351,#5352);
#4453=AXIS2_PLACEMENT_3D('',#6612,#5353,#5354);
#4454=AXIS2_PLACEMENT_3D('',#6613,#5355,#5356);
#4455=AXIS2_PLACEMENT_3D('',#6614,#5357,#5358);
#4456=AXIS2_PLACEMENT_3D('',#6615,#5359,#5360);
#4457=AXIS2_PLACEMENT_3D('',#6616,#5361,#5362);
#4458=AXIS2_PLACEMENT_3D('',#6617,#5363,#5364);
#4459=AXIS2_PLACEMENT_3D('',#6618,#5365,#5366);
#4460=AXIS2_PLACEMENT_3D('',#6619,#5367,#5368);
#4461=AXIS2_PLACEMENT_3D('',#6621,#5369,#5370);
#4462=AXIS2_PLACEMENT_3D('',#6624,#5372,#5373);
#4463=AXIS2_PLACEMENT_3D('',#6625,#5374,#5375);
#4464=AXIS2_PLACEMENT_3D('',#6627,#5376,#5377);
#4465=AXIS2_PLACEMENT_3D('',#6630,#5379,#5380);
#4466=AXIS2_PLACEMENT_3D('',#6631,#5381,#5382);
#4467=AXIS2_PLACEMENT_3D('',#6633,#5383,#5384);
#4468=AXIS2_PLACEMENT_3D('',#6636,#5386,#5387);
#4469=AXIS2_PLACEMENT_3D('',#6637,#5388,#5389);
#4470=AXIS2_PLACEMENT_3D('',#6639,#5390,#5391);
#4471=AXIS2_PLACEMENT_3D('',#6642,#5393,#5394);
#4472=AXIS2_PLACEMENT_3D('',#6643,#5395,#5396);
#4473=AXIS2_PLACEMENT_3D('',#6645,#5397,#5398);
#4474=AXIS2_PLACEMENT_3D('',#6648,#5400,#5401);
#4475=AXIS2_PLACEMENT_3D('',#6649,#5402,#5403);
#4476=AXIS2_PLACEMENT_3D('',#6651,#5404,#5405);
#4477=AXIS2_PLACEMENT_3D('',#6653,#5407,#5408);
#4478=AXIS2_PLACEMENT_3D('',#6655,#5409,#5410);
#4479=AXIS2_PLACEMENT_3D('',#6657,#5412,#5413);
#4480=AXIS2_PLACEMENT_3D('',#6659,#5414,#5415);
#4481=AXIS2_PLACEMENT_3D('',#6660,#5416,#5417);
#4482=AXIS2_PLACEMENT_3D('',#6662,#5418,#5419);
#4483=AXIS2_PLACEMENT_3D('',#6664,#5420,#5421);
#4484=AXIS2_PLACEMENT_3D('',#6665,#5422,#5423);
#4485=AXIS2_PLACEMENT_3D('',#6667,#5425,#5426);
#4486=AXIS2_PLACEMENT_3D('',#6670,#5428,#5429);
#4487=AXIS2_PLACEMENT_3D('',#6671,#5430,#5431);
#4488=AXIS2_PLACEMENT_3D('',#6673,#5432,#5433);
#4489=AXIS2_PLACEMENT_3D('',#6676,#5435,#5436);
#4490=AXIS2_PLACEMENT_3D('',#6677,#5437,#5438);
#4491=AXIS2_PLACEMENT_3D('',#6679,#5439,#5440);
#4492=AXIS2_PLACEMENT_3D('',#6681,#5442,#5443);
#4493=AXIS2_PLACEMENT_3D('',#6682,#5444,#5445);
#4494=AXIS2_PLACEMENT_3D('',#6683,#5446,#5447);
#4495=AXIS2_PLACEMENT_3D('',#6684,#5448,#5449);
#4496=AXIS2_PLACEMENT_3D('',#6686,#5450,#5451);
#4497=AXIS2_PLACEMENT_3D('',#6689,#5453,#5454);
#4498=AXIS2_PLACEMENT_3D('',#6690,#5455,#5456);
#4499=AXIS2_PLACEMENT_3D('',#6692,#5457,#5458);
#4500=AXIS2_PLACEMENT_3D('',#6695,#5460,#5461);
#4501=AXIS2_PLACEMENT_3D('',#6696,#5462,#5463);
#4502=AXIS2_PLACEMENT_3D('',#6697,#5464,#5465);
#4503=AXIS2_PLACEMENT_3D('',#6698,#5466,#5467);
#4504=AXIS2_PLACEMENT_3D('',#6699,#5468,#5469);
#4505=AXIS2_PLACEMENT_3D('',#6700,#5470,#5471);
#4506=AXIS2_PLACEMENT_3D('',#6703,#5472,#5473);
#4507=AXIS2_PLACEMENT_3D('',#6704,#5474,#5475);
#4508=AXIS2_PLACEMENT_3D('',#6706,#5476,#5477);
#4509=AXIS2_PLACEMENT_3D('',#6708,#5478,#5479);
#4510=AXIS2_PLACEMENT_3D('',#6709,#5480,#5481);
#4511=AXIS2_PLACEMENT_3D('',#6710,#5482,#5483);
#4512=AXIS2_PLACEMENT_3D('',#6713,#5485,#5486);
#4513=AXIS2_PLACEMENT_3D('',#6714,#5487,#5488);
#4514=AXIS2_PLACEMENT_3D('',#6716,#5489,#5490);
#4515=AXIS2_PLACEMENT_3D('',#6719,#5492,#5493);
#4516=AXIS2_PLACEMENT_3D('',#6720,#5494,#5495);
#4517=AXIS2_PLACEMENT_3D('',#6723,#5497,#5498);
#4518=AXIS2_PLACEMENT_3D('',#6724,#5499,#5500);
#4519=AXIS2_PLACEMENT_3D('',#6725,#5501,#5502);
#4520=AXIS2_PLACEMENT_3D('',#6727,#5503,#5504);
#4521=AXIS2_PLACEMENT_3D('',#6729,#5506,#5507);
#4522=AXIS2_PLACEMENT_3D('',#6731,#5508,#5509);
#4523=AXIS2_PLACEMENT_3D('',#6732,#5510,#5511);
#4524=AXIS2_PLACEMENT_3D('',#6734,#5513,#5514);
#4525=AXIS2_PLACEMENT_3D('',#6735,#5515,#5516);
#4526=AXIS2_PLACEMENT_3D('',#6738,#5517,#5518);
#4527=AXIS2_PLACEMENT_3D('',#6739,#5519,#5520);
#4528=AXIS2_PLACEMENT_3D('',#6741,#5521,#5522);
#4529=AXIS2_PLACEMENT_3D('',#6743,#5523,#5524);
#4530=AXIS2_PLACEMENT_3D('',#6744,#5525,#5526);
#4531=AXIS2_PLACEMENT_3D('',#6745,#5527,#5528);
#4532=AXIS2_PLACEMENT_3D('',#6747,#5529,#5530);
#4533=AXIS2_PLACEMENT_3D('',#6749,#5532,#5533);
#4534=AXIS2_PLACEMENT_3D('',#6751,#5534,#5535);
#4535=AXIS2_PLACEMENT_3D('',#6753,#5536,#5537);
#4536=AXIS2_PLACEMENT_3D('',#6754,#5538,#5539);
#4537=AXIS2_PLACEMENT_3D('',#6756,#5540,#5541);
#4538=AXIS2_PLACEMENT_3D('',#6758,#5543,#5544);
#4539=AXIS2_PLACEMENT_3D('',#6760,#5545,#5546);
#4540=AXIS2_PLACEMENT_3D('',#6762,#5548,#5549);
#4541=AXIS2_PLACEMENT_3D('',#6764,#5550,#5551);
#4542=AXIS2_PLACEMENT_3D('',#6766,#5553,#5554);
#4543=AXIS2_PLACEMENT_3D('',#6767,#5555,#5556);
#4544=AXIS2_PLACEMENT_3D('',#6769,#5558,#5559);
#4545=AXIS2_PLACEMENT_3D('',#6770,#5560,#5561);
#4546=AXIS2_PLACEMENT_3D('',#6773,#5562,#5563);
#4547=AXIS2_PLACEMENT_3D('',#6774,#5564,#5565);
#4548=AXIS2_PLACEMENT_3D('',#6777,#5566,#5567);
#4549=AXIS2_PLACEMENT_3D('',#6778,#5568,#5569);
#4550=AXIS2_PLACEMENT_3D('',#6781,#5570,#5571);
#4551=AXIS2_PLACEMENT_3D('',#6782,#5572,#5573);
#4552=AXIS2_PLACEMENT_3D('',#6785,#5574,#5575);
#4553=AXIS2_PLACEMENT_3D('',#6786,#5576,#5577);
#4554=AXIS2_PLACEMENT_3D('',#6789,#5578,#5579);
#4555=AXIS2_PLACEMENT_3D('',#6790,#5580,#5581);
#4556=AXIS2_PLACEMENT_3D('',#6793,#5582,#5583);
#4557=AXIS2_PLACEMENT_3D('',#6794,#5584,#5585);
#4558=AXIS2_PLACEMENT_3D('',#6797,#5586,#5587);
#4559=AXIS2_PLACEMENT_3D('',#6798,#5588,#5589);
#4560=AXIS2_PLACEMENT_3D('',#6801,#5590,#5591);
#4561=AXIS2_PLACEMENT_3D('',#6802,#5592,#5593);
#4562=AXIS2_PLACEMENT_3D('',#6803,#5594,#5595);
#4563=AXIS2_PLACEMENT_3D('',#6829,#5596,#5597);
#4564=AXIS2_PLACEMENT_3D('',#6853,#5598,#5599);
#4565=AXIS2_PLACEMENT_3D('',#6854,#5600,#5601);
#4566=AXIS2_PLACEMENT_3D('',#6856,#5602,#5603);
#4567=AXIS2_PLACEMENT_3D('',#6881,#5604,#5605);
#4568=AXIS2_PLACEMENT_3D('',#6906,#5606,#5607);
#4569=AXIS2_PLACEMENT_3D('',#6922,#5609,#5610);
#4570=AXIS2_PLACEMENT_3D('',#6937,#5611,#5612);
#4571=AXIS2_PLACEMENT_3D('',#6962,#5613,#5614);
#4572=AXIS2_PLACEMENT_3D('',#6987,#5615,#5616);
#4573=AXIS2_PLACEMENT_3D('',#7012,#5617,#5618);
#4574=AXIS2_PLACEMENT_3D('',#7036,#5619,#5620);
#4575=AXIS2_PLACEMENT_3D('',#7037,#5621,#5622);
#4576=AXIS2_PLACEMENT_3D('',#7039,#5623,#5624);
#4577=AXIS2_PLACEMENT_3D('',#7040,#5625,#5626);
#4578=AXIS2_PLACEMENT_3D('',#7041,#5627,#5628);
#4579=AXIS2_PLACEMENT_3D('',#7065,#5629,#5630);
#4580=AXIS2_PLACEMENT_3D('',#7066,#5631,#5632);
#4581=AXIS2_PLACEMENT_3D('',#7068,#5633,#5634);
#4582=AXIS2_PLACEMENT_3D('',#7069,#5635,#5636);
#4583=AXIS2_PLACEMENT_3D('',#7070,#5637,#5638);
#4584=AXIS2_PLACEMENT_3D('',#7094,#5639,#5640);
#4585=AXIS2_PLACEMENT_3D('',#7095,#5641,#5642);
#4586=AXIS2_PLACEMENT_3D('',#7097,#5643,#5644);
#4587=AXIS2_PLACEMENT_3D('',#7098,#5645,#5646);
#4588=AXIS2_PLACEMENT_3D('',#7099,#5647,#5648);
#4589=AXIS2_PLACEMENT_3D('',#7114,#5649,#5650);
#4590=AXIS2_PLACEMENT_3D('',#7127,#5651,#5652);
#4591=AXIS2_PLACEMENT_3D('',#7129,#5653,#5654);
#4592=AXIS2_PLACEMENT_3D('',#7130,#5655,#5656);
#4593=AXIS2_PLACEMENT_3D('',#7131,#5657,#5658);
#4594=AXIS2_PLACEMENT_3D('',#7155,#5659,#5660);
#4595=AXIS2_PLACEMENT_3D('',#7156,#5661,#5662);
#4596=AXIS2_PLACEMENT_3D('',#7158,#5663,#5664);
#4597=AXIS2_PLACEMENT_3D('',#7159,#5665,#5666);
#4598=AXIS2_PLACEMENT_3D('',#7160,#5667,#5668);
#4599=AXIS2_PLACEMENT_3D('',#7184,#5669,#5670);
#4600=AXIS2_PLACEMENT_3D('',#7185,#5671,#5672);
#4601=AXIS2_PLACEMENT_3D('',#7187,#5673,#5674);
#4602=AXIS2_PLACEMENT_3D('',#7188,#5675,#5676);
#4603=AXIS2_PLACEMENT_3D('',#7189,#5677,#5678);
#4604=AXIS2_PLACEMENT_3D('',#7213,#5679,#5680);
#4605=AXIS2_PLACEMENT_3D('',#7214,#5681,#5682);
#4606=AXIS2_PLACEMENT_3D('',#7216,#5683,#5684);
#4607=AXIS2_PLACEMENT_3D('',#7219,#5686,#5687);
#4608=AXIS2_PLACEMENT_3D('',#7243,#5688,#5689);
#4609=AXIS2_PLACEMENT_3D('',#7244,#5690,#5691);
#4610=AXIS2_PLACEMENT_3D('',#7245,#5692,#5693);
#4611=AXIS2_PLACEMENT_3D('',#7246,#5694,#5695);
#4612=AXIS2_PLACEMENT_3D('',#7247,#5696,#5697);
#4613=AXIS2_PLACEMENT_3D('',#7248,#5698,#5699);
#4614=AXIS2_PLACEMENT_3D('',#7249,#5700,#5701);
#4615=AXIS2_PLACEMENT_3D('',#7250,#5702,#5703);
#4616=AXIS2_PLACEMENT_3D('',#7251,#5704,#5705);
#4617=AXIS2_PLACEMENT_3D('',#7253,#5706,#5707);
#4618=AXIS2_PLACEMENT_3D('',#7255,#5708,#5709);
#4619=AXIS2_PLACEMENT_3D('',#7256,#5710,#5711);
#4620=AXIS2_PLACEMENT_3D('',#7258,#5712,#5713);
#4621=AXIS2_PLACEMENT_3D('',#7260,#5715,#5716);
#4622=AXIS2_PLACEMENT_3D('',#7262,#5717,#5718);
#4623=AXIS2_PLACEMENT_3D('',#7263,#5719,#5720);
#4624=AXIS2_PLACEMENT_3D('',#7265,#5722,#5723);
#4625=AXIS2_PLACEMENT_3D('',#7267,#5724,#5725);
#4626=AXIS2_PLACEMENT_3D('',#7269,#5726,#5727);
#4627=AXIS2_PLACEMENT_3D('',#7270,#5728,#5729);
#4628=AXIS2_PLACEMENT_3D('',#7272,#5730,#5731);
#4629=AXIS2_PLACEMENT_3D('',#7274,#5733,#5734);
#4630=AXIS2_PLACEMENT_3D('',#7276,#5735,#5736);
#4631=AXIS2_PLACEMENT_3D('',#7277,#5737,#5738);
#4632=AXIS2_PLACEMENT_3D('',#7279,#5740,#5741);
#4633=AXIS2_PLACEMENT_3D('',#7280,#5742,#5743);
#4634=AXIS2_PLACEMENT_3D('',#7281,#5744,#5745);
#4635=AXIS2_PLACEMENT_3D('',#7282,#5746,#5747);
#4636=AXIS2_PLACEMENT_3D('',#7283,#5748,#5749);
#4637=AXIS2_PLACEMENT_3D('',#7284,#5750,#5751);
#4638=AXIS2_PLACEMENT_3D('',#7285,#5752,#5753);
#4639=AXIS2_PLACEMENT_3D('',#7287,#5754,#5755);
#4640=AXIS2_PLACEMENT_3D('',#7290,#5757,#5758);
#4641=AXIS2_PLACEMENT_3D('',#7291,#5759,#5760);
#4642=AXIS2_PLACEMENT_3D('',#7293,#5761,#5762);
#4643=AXIS2_PLACEMENT_3D('',#7296,#5764,#5765);
#4644=AXIS2_PLACEMENT_3D('',#7297,#5766,#5767);
#4645=AXIS2_PLACEMENT_3D('',#7299,#5768,#5769);
#4646=AXIS2_PLACEMENT_3D('',#7302,#5771,#5772);
#4647=AXIS2_PLACEMENT_3D('',#7303,#5773,#5774);
#4648=AXIS2_PLACEMENT_3D('',#7305,#5775,#5776);
#4649=AXIS2_PLACEMENT_3D('',#7308,#5778,#5779);
#4650=AXIS2_PLACEMENT_3D('',#7309,#5780,#5781);
#4651=AXIS2_PLACEMENT_3D('',#7311,#5782,#5783);
#4652=AXIS2_PLACEMENT_3D('',#7314,#5785,#5786);
#4653=AXIS2_PLACEMENT_3D('',#7315,#5787,#5788);
#4654=AXIS2_PLACEMENT_3D('',#7317,#5789,#5790);
#4655=AXIS2_PLACEMENT_3D('',#7318,#5791,#5792);
#4656=AXIS2_PLACEMENT_3D('',#7321,#5794,#5795);
#4657=AXIS2_PLACEMENT_3D('',#7322,#5796,#5797);
#4658=AXIS2_PLACEMENT_3D('',#7324,#5798,#5799);
#4659=AXIS2_PLACEMENT_3D('',#7327,#5801,#5802);
#4660=AXIS2_PLACEMENT_3D('',#7328,#5803,#5804);
#4661=AXIS2_PLACEMENT_3D('',#7329,#5805,#5806);
#4662=AXIS2_PLACEMENT_3D('',#7330,#5807,#5808);
#4663=AXIS2_PLACEMENT_3D('',#7331,#5809,#5810);
#4664=AXIS2_PLACEMENT_3D('',#7340,#5815,#5816);
#4665=AXIS2_PLACEMENT_3D('',#7346,#5820,#5821);
#4666=AXIS2_PLACEMENT_3D('',#7352,#5825,#5826);
#4667=AXIS2_PLACEMENT_3D('',#7358,#5830,#5831);
#4668=AXIS2_PLACEMENT_3D('',#7364,#5835,#5836);
#4669=AXIS2_PLACEMENT_3D('',#7367,#5839,#5840);
#4670=AXIS2_PLACEMENT_3D('',#7368,#5841,#5842);
#4671=AXIS2_PLACEMENT_3D('',#7369,#5843,#5844);
#4672=AXIS2_PLACEMENT_3D('',#7371,#5845,#5846);
#4673=AXIS2_PLACEMENT_3D('',#7372,#5847,#5848);
#4674=AXIS2_PLACEMENT_3D('',#7374,#5849,#5850);
#4675=AXIS2_PLACEMENT_3D('',#7375,#5851,#5852);
#4676=AXIS2_PLACEMENT_3D('',#7377,#5853,#5854);
#4677=AXIS2_PLACEMENT_3D('',#7379,#5856,#5857);
#4678=AXIS2_PLACEMENT_3D('',#7381,#5858,#5859);
#4679=AXIS2_PLACEMENT_3D('',#7383,#5861,#5862);
#4680=AXIS2_PLACEMENT_3D('',#7385,#5863,#5864);
#4681=AXIS2_PLACEMENT_3D('',#7387,#5866,#5867);
#4682=AXIS2_PLACEMENT_3D('',#7389,#5868,#5869);
#4683=AXIS2_PLACEMENT_3D('',#7390,#5870,#5871);
#4684=AXIS2_PLACEMENT_3D('',#7392,#5872,#5873);
#4685=AXIS2_PLACEMENT_3D('',#7394,#5875,#5876);
#4686=AXIS2_PLACEMENT_3D('',#7396,#5878,#5879);
#4687=AXIS2_PLACEMENT_3D('',#7397,#5880,#5881);
#4688=AXIS2_PLACEMENT_3D('',#7398,#5882,#5883);
#4689=AXIS2_PLACEMENT_3D('',#7399,#5884,#5885);
#4690=AXIS2_PLACEMENT_3D('',#7400,#5886,#5887);
#4691=AXIS2_PLACEMENT_3D('',#7401,#5888,#5889);
#4692=AXIS2_PLACEMENT_3D('',#7402,#5890,#5891);
#4693=AXIS2_PLACEMENT_3D('',#7403,#5892,#5893);
#4694=AXIS2_PLACEMENT_3D('',#7404,#5894,#5895);
#4695=AXIS2_PLACEMENT_3D('',#7405,#5896,#5897);
#4696=AXIS2_PLACEMENT_3D('',#7406,#5898,#5899);
#4697=AXIS2_PLACEMENT_3D('',#7407,#5900,#5901);
#4698=AXIS2_PLACEMENT_3D('',#7408,#5902,#5903);
#4699=AXIS2_PLACEMENT_3D('',#7409,#5904,#5905);
#4700=AXIS2_PLACEMENT_3D('',#7410,#5906,#5907);
#4701=AXIS2_PLACEMENT_3D('',#7411,#5908,#5909);
#4702=AXIS2_PLACEMENT_3D('',#7412,#5910,#5911);
#4703=AXIS2_PLACEMENT_3D('',#7414,#5912,#5913);
#4704=AXIS2_PLACEMENT_3D('',#7416,#5914,#5915);
#4705=AXIS2_PLACEMENT_3D('',#7417,#5916,#5917);
#4706=AXIS2_PLACEMENT_3D('',#7419,#5918,#5919);
#4707=AXIS2_PLACEMENT_3D('',#7421,#5920,#5921);
#4708=AXIS2_PLACEMENT_3D('',#7422,#5922,#5923);
#4709=AXIS2_PLACEMENT_3D('',#7424,#5925,#5926);
#4710=AXIS2_PLACEMENT_3D('',#7428,#5928,#5929);
#4711=AXIS2_PLACEMENT_3D('',#7430,#5930,#5931);
#4712=AXIS2_PLACEMENT_3D('',#7431,#5932,#5933);
#4713=AXIS2_PLACEMENT_3D('',#7432,#5934,#5935);
#4714=AXIS2_PLACEMENT_3D('',#7434,#5936,#5937);
#4715=AXIS2_PLACEMENT_3D('',#7436,#5939,#5940);
#4716=AXIS2_PLACEMENT_3D('',#7437,#5941,#5942);
#4717=AXIS2_PLACEMENT_3D('',#7443,#5946,#5947);
#4718=AXIS2_PLACEMENT_3D('',#7449,#5951,#5952);
#4719=AXIS2_PLACEMENT_3D('',#7455,#5956,#5957);
#4720=AXIS2_PLACEMENT_3D('',#7464,#5962,#5963);
#4721=AXIS2_PLACEMENT_3D('',#7467,#5965,#5966);
#4722=AXIS2_PLACEMENT_3D('',#7470,#5968,#5969);
#4723=AXIS2_PLACEMENT_3D('',#7471,#5970,#5971);
#4724=AXIS2_PLACEMENT_3D('',#7473,#5972,#5973);
#4725=AXIS2_PLACEMENT_3D('',#7475,#5975,#5976);
#4726=AXIS2_PLACEMENT_3D('',#7478,#5978,#5979);
#4727=AXIS2_PLACEMENT_3D('',#7480,#5981,#5982);
#4728=AXIS2_PLACEMENT_3D('',#7481,#5983,#5984);
#4729=AXIS2_PLACEMENT_3D('',#7483,#5986,#5987);
#4730=AXIS2_PLACEMENT_3D('',#7484,#5988,#5989);
#4731=AXIS2_PLACEMENT_3D('',#7485,#5990,#5991);
#4732=AXIS2_PLACEMENT_3D('',#7487,#5992,#5993);
#4733=AXIS2_PLACEMENT_3D('',#7490,#5995,#5996);
#4734=AXIS2_PLACEMENT_3D('',#7491,#5997,#5998);
#4735=AXIS2_PLACEMENT_3D('',#7493,#5999,#6000);
#4736=AXIS2_PLACEMENT_3D('',#7496,#6002,#6003);
#4737=AXIS2_PLACEMENT_3D('',#7497,#6004,#6005);
#4738=AXIS2_PLACEMENT_3D('',#7498,#6006,#6007);
#4739=AXIS2_PLACEMENT_3D('',#7499,#6008,#6009);
#4740=AXIS2_PLACEMENT_3D('',#7500,#6010,#6011);
#4741=AXIS2_PLACEMENT_3D('',#7502,#6012,#6013);
#4742=AXIS2_PLACEMENT_3D('',#7505,#6015,#6016);
#4743=AXIS2_PLACEMENT_3D('',#7506,#6017,#6018);
#4744=AXIS2_PLACEMENT_3D('',#7515,#6023,#6024);
#4745=AXIS2_PLACEMENT_3D('',#7521,#6028,#6029);
#4746=AXIS2_PLACEMENT_3D('',#7527,#6033,#6034);
#4747=AXIS2_PLACEMENT_3D('',#7533,#6038,#6039);
#4748=AXIS2_PLACEMENT_3D('',#7539,#6043,#6044);
#4749=AXIS2_PLACEMENT_3D('',#7542,#6047,#6048);
#4750=AXIS2_PLACEMENT_3D('',#7543,#6049,#6050);
#4751=AXIS2_PLACEMENT_3D('',#7544,#6051,#6052);
#4752=AXIS2_PLACEMENT_3D('',#7545,#6053,#6054);
#4753=AXIS2_PLACEMENT_3D('',#7546,#6055,#6056);
#4754=AXIS2_PLACEMENT_3D('',#7547,#6057,#6058);
#4755=AXIS2_PLACEMENT_3D('',#7548,#6059,#6060);
#4756=AXIS2_PLACEMENT_3D('',#7549,#6061,#6062);
#4757=DIRECTION('axis',(0.,0.,1.));
#4758=DIRECTION('refdir',(1.,0.,0.));
#4759=DIRECTION('axis',(0.,0.,1.));
#4760=DIRECTION('refdir',(1.,0.,0.));
#4761=DIRECTION('axis',(0.,0.,1.));
#4762=DIRECTION('refdir',(1.,0.,0.));
#4763=DIRECTION('center_axis',(0.,1.,0.));
#4764=DIRECTION('ref_axis',(1.,0.,0.));
#4765=DIRECTION('center_axis',(0.,1.,0.));
#4766=DIRECTION('ref_axis',(1.,0.,0.));
#4767=DIRECTION('center_axis',(0.,1.,0.));
#4768=DIRECTION('ref_axis',(1.,0.,0.));
#4769=DIRECTION('center_axis',(0.,1.,0.));
#4770=DIRECTION('ref_axis',(1.,0.,0.));
#4771=DIRECTION('center_axis',(0.,1.,0.));
#4772=DIRECTION('ref_axis',(1.,0.,0.));
#4773=DIRECTION('center_axis',(0.,1.,0.));
#4774=DIRECTION('ref_axis',(1.,0.,0.));
#4775=DIRECTION('center_axis',(0.,1.,0.));
#4776=DIRECTION('ref_axis',(1.,0.,0.));
#4777=DIRECTION('center_axis',(0.,1.,0.));
#4778=DIRECTION('ref_axis',(1.,0.,0.));
#4779=DIRECTION('center_axis',(0.,1.,0.));
#4780=DIRECTION('ref_axis',(1.,0.,0.));
#4781=DIRECTION('center_axis',(0.,-1.,0.));
#4782=DIRECTION('ref_axis',(1.,0.,0.));
#4783=DIRECTION('center_axis',(0.,1.,0.));
#4784=DIRECTION('ref_axis',(1.,0.,0.));
#4785=DIRECTION('',(0.,1.,0.));
#4786=DIRECTION('',(0.,-1.,0.));
#4787=DIRECTION('center_axis',(0.,-1.,0.));
#4788=DIRECTION('ref_axis',(1.,0.,0.));
#4789=DIRECTION('center_axis',(0.,1.,0.));
#4790=DIRECTION('ref_axis',(1.,0.,0.));
#4791=DIRECTION('',(0.,-1.,0.));
#4792=DIRECTION('center_axis',(0.,-1.,0.));
#4793=DIRECTION('ref_axis',(1.,0.,0.));
#4794=DIRECTION('',(0.,1.,0.));
#4795=DIRECTION('center_axis',(0.,1.,0.));
#4796=DIRECTION('ref_axis',(1.,0.,0.));
#4797=DIRECTION('',(0.,1.,0.));
#4798=DIRECTION('',(0.,-1.,0.));
#4799=DIRECTION('center_axis',(0.,-1.,0.));
#4800=DIRECTION('ref_axis',(1.,0.,0.));
#4801=DIRECTION('center_axis',(0.,1.,0.));
#4802=DIRECTION('ref_axis',(1.,0.,0.));
#4803=DIRECTION('',(0.,1.,0.));
#4804=DIRECTION('center_axis',(0.,1.,0.));
#4805=DIRECTION('ref_axis',(1.,0.,0.));
#4806=DIRECTION('center_axis',(0.,1.,0.));
#4807=DIRECTION('ref_axis',(-1.,0.,-1.22464679914735E-16));
#4808=DIRECTION('',(0.,-1.,0.));
#4809=DIRECTION('center_axis',(0.,-1.,0.));
#4810=DIRECTION('ref_axis',(1.,0.,0.));
#4811=DIRECTION('',(0.,1.,0.));
#4812=DIRECTION('center_axis',(0.,1.,0.));
#4813=DIRECTION('ref_axis',(1.,0.,0.));
#4814=DIRECTION('center_axis',(0.,1.,0.));
#4815=DIRECTION('ref_axis',(1.,0.,0.));
#4816=DIRECTION('',(0.,1.,0.));
#4817=DIRECTION('center_axis',(0.,-1.,0.));
#4818=DIRECTION('ref_axis',(1.,0.,0.));
#4819=DIRECTION('center_axis',(0.,-1.,0.));
#4820=DIRECTION('ref_axis',(1.,0.,0.));
#4821=DIRECTION('center_axis',(0.,1.,0.));
#4822=DIRECTION('ref_axis',(1.,0.,0.));
#4823=DIRECTION('center_axis',(0.,1.,0.));
#4824=DIRECTION('ref_axis',(1.,0.,0.));
#4825=DIRECTION('',(0.,1.,0.));
#4826=DIRECTION('center_axis',(0.,-1.,0.));
#4827=DIRECTION('ref_axis',(1.,0.,0.));
#4828=DIRECTION('center_axis',(0.,-1.,0.));
#4829=DIRECTION('ref_axis',(1.,0.,0.));
#4830=DIRECTION('center_axis',(0.,1.,0.));
#4831=DIRECTION('ref_axis',(1.,0.,0.));
#4832=DIRECTION('center_axis',(0.,1.,0.));
#4833=DIRECTION('ref_axis',(1.,0.,0.));
#4834=DIRECTION('',(0.,1.,0.));
#4835=DIRECTION('center_axis',(0.,-1.,0.));
#4836=DIRECTION('ref_axis',(1.,0.,0.));
#4837=DIRECTION('center_axis',(0.,-1.,0.));
#4838=DIRECTION('ref_axis',(1.,0.,0.));
#4839=DIRECTION('center_axis',(0.,1.,0.));
#4840=DIRECTION('ref_axis',(0.,0.,1.));
#4841=DIRECTION('center_axis',(0.,-1.,0.));
#4842=DIRECTION('ref_axis',(1.,0.,0.));
#4843=DIRECTION('center_axis',(0.,1.,0.));
#4844=DIRECTION('ref_axis',(1.,0.,0.));
#4845=DIRECTION('center_axis',(0.,1.,0.));
#4846=DIRECTION('ref_axis',(1.,0.,0.));
#4847=DIRECTION('',(0.,1.,0.));
#4848=DIRECTION('center_axis',(0.,-1.,0.));
#4849=DIRECTION('ref_axis',(1.,0.,0.));
#4850=DIRECTION('center_axis',(0.,-1.,0.));
#4851=DIRECTION('ref_axis',(1.,0.,0.));
#4852=DIRECTION('center_axis',(0.,1.,0.));
#4853=DIRECTION('ref_axis',(1.,0.,0.));
#4854=DIRECTION('center_axis',(0.,1.,0.));
#4855=DIRECTION('ref_axis',(1.,0.,0.));
#4856=DIRECTION('',(0.,1.,0.));
#4857=DIRECTION('center_axis',(0.,-1.,0.));
#4858=DIRECTION('ref_axis',(1.,0.,0.));
#4859=DIRECTION('center_axis',(0.,1.,0.));
#4860=DIRECTION('ref_axis',(1.,0.,0.));
#4861=DIRECTION('center_axis',(0.,1.,0.));
#4862=DIRECTION('ref_axis',(1.,0.,0.));
#4863=DIRECTION('',(0.,1.,0.));
#4864=DIRECTION('center_axis',(0.,-1.,0.));
#4865=DIRECTION('ref_axis',(1.,0.,0.));
#4866=DIRECTION('center_axis',(0.,1.,0.));
#4867=DIRECTION('ref_axis',(1.,0.,0.));
#4868=DIRECTION('center_axis',(0.,1.,0.));
#4869=DIRECTION('ref_axis',(1.,0.,0.));
#4870=DIRECTION('',(0.,1.,0.));
#4871=DIRECTION('center_axis',(0.,-1.,0.));
#4872=DIRECTION('ref_axis',(1.,0.,0.));
#4873=DIRECTION('center_axis',(0.,1.,0.));
#4874=DIRECTION('ref_axis',(1.,0.,0.));
#4875=DIRECTION('center_axis',(0.,1.,0.));
#4876=DIRECTION('ref_axis',(1.,0.,0.));
#4877=DIRECTION('',(0.,1.,0.));
#4878=DIRECTION('center_axis',(-0.832050294337844,0.,-0.554700196225229));
#4879=DIRECTION('ref_axis',(-0.554700196225229,0.,0.832050294337844));
#4880=DIRECTION('',(0.554700196225229,0.,-0.832050294337844));
#4881=DIRECTION('',(0.,1.,0.));
#4882=DIRECTION('',(-0.554700196225229,0.,0.832050294337844));
#4883=DIRECTION('',(0.,1.,0.));
#4884=DIRECTION('center_axis',(0.,0.,-1.));
#4885=DIRECTION('ref_axis',(-1.,0.,0.));
#4886=DIRECTION('',(1.,0.,0.));
#4887=DIRECTION('',(-1.,0.,0.));
#4888=DIRECTION('',(0.,1.,0.));
#4889=DIRECTION('center_axis',(0.832050294337844,0.,-0.554700196225229));
#4890=DIRECTION('ref_axis',(-0.554700196225229,0.,-0.832050294337844));
#4891=DIRECTION('',(0.554700196225229,0.,0.832050294337844));
#4892=DIRECTION('',(-0.554700196225229,0.,-0.832050294337844));
#4893=DIRECTION('',(0.,1.,0.));
#4894=DIRECTION('center_axis',(1.,0.,0.));
#4895=DIRECTION('ref_axis',(0.,0.,-1.));
#4896=DIRECTION('',(0.,0.,1.));
#4897=DIRECTION('',(0.,0.,-1.));
#4898=DIRECTION('',(0.,1.,0.));
#4899=DIRECTION('center_axis',(0.894427190999916,0.,0.447213595499958));
#4900=DIRECTION('ref_axis',(0.447213595499958,0.,-0.894427190999916));
#4901=DIRECTION('',(-0.447213595499958,0.,0.894427190999916));
#4902=DIRECTION('',(0.447213595499958,0.,-0.894427190999916));
#4903=DIRECTION('',(0.,1.,0.));
#4904=DIRECTION('center_axis',(0.,0.,1.));
#4905=DIRECTION('ref_axis',(1.,0.,0.));
#4906=DIRECTION('',(-1.,0.,0.));
#4907=DIRECTION('',(1.,0.,0.));
#4908=DIRECTION('',(0.,1.,0.));
#4909=DIRECTION('center_axis',(-0.894427190999916,0.,0.447213595499958));
#4910=DIRECTION('ref_axis',(0.447213595499958,0.,0.894427190999916));
#4911=DIRECTION('',(-0.447213595499958,0.,-0.894427190999916));
#4912=DIRECTION('',(0.447213595499958,0.,0.894427190999916));
#4913=DIRECTION('',(0.,1.,0.));
#4914=DIRECTION('center_axis',(-1.,0.,0.));
#4915=DIRECTION('ref_axis',(0.,0.,1.));
#4916=DIRECTION('',(0.,0.,-1.));
#4917=DIRECTION('',(0.,0.,1.));
#4918=DIRECTION('center_axis',(0.,1.,0.));
#4919=DIRECTION('ref_axis',(0.,0.,1.));
#4920=DIRECTION('center_axis',(0.,1.,0.));
#4921=DIRECTION('ref_axis',(1.,0.,0.));
#4922=DIRECTION('axis',(0.,0.,1.));
#4923=DIRECTION('refdir',(1.,0.,0.));
#4924=DIRECTION('center_axis',(0.,0.,1.));
#4925=DIRECTION('ref_axis',(1.,0.,0.));
#4926=DIRECTION('center_axis',(0.,0.,1.));
#4927=DIRECTION('ref_axis',(1.,0.,0.));
#4928=DIRECTION('',(0.,0.,1.));
#4929=DIRECTION('center_axis',(0.,0.,-1.));
#4930=DIRECTION('ref_axis',(1.,0.,0.));
#4931=DIRECTION('center_axis',(0.,1.,0.));
#4932=DIRECTION('ref_axis',(1.,0.,0.));
#4933=DIRECTION('center_axis',(0.,1.,0.));
#4934=DIRECTION('ref_axis',(1.,0.,0.));
#4935=DIRECTION('',(0.,1.,0.));
#4936=DIRECTION('center_axis',(0.,-1.,0.));
#4937=DIRECTION('ref_axis',(1.,0.,0.));
#4938=DIRECTION('center_axis',(0.,1.,0.));
#4939=DIRECTION('ref_axis',(1.,0.,0.));
#4940=DIRECTION('center_axis',(0.,1.,0.));
#4941=DIRECTION('ref_axis',(1.,0.,0.));
#4942=DIRECTION('',(0.,1.,0.));
#4943=DIRECTION('center_axis',(0.,-1.,0.));
#4944=DIRECTION('ref_axis',(1.,0.,0.));
#4945=DIRECTION('center_axis',(0.,1.,0.));
#4946=DIRECTION('ref_axis',(-1.,0.,0.));
#4947=DIRECTION('',(-1.,0.,0.));
#4948=DIRECTION('',(0.,0.,1.));
#4949=DIRECTION('',(-1.,0.,0.));
#4950=DIRECTION('',(0.,0.,1.));
#4951=DIRECTION('center_axis',(1.,0.,0.));
#4952=DIRECTION('ref_axis',(0.,1.,0.));
#4953=DIRECTION('',(0.,1.,0.));
#4954=DIRECTION('',(0.,1.,0.));
#4955=DIRECTION('',(0.,0.,1.));
#4956=DIRECTION('center_axis',(0.,-1.,0.));
#4957=DIRECTION('ref_axis',(1.,0.,0.));
#4958=DIRECTION('',(1.,0.,0.));
#4959=DIRECTION('',(1.,0.,0.));
#4960=DIRECTION('',(0.,0.,1.));
#4961=DIRECTION('center_axis',(-1.,0.,0.));
#4962=DIRECTION('ref_axis',(0.,-1.,0.));
#4963=DIRECTION('',(0.,-1.,0.));
#4964=DIRECTION('',(0.,-1.,0.));
#4965=DIRECTION('center_axis',(0.,0.,1.));
#4966=DIRECTION('ref_axis',(1.,0.,0.));
#4967=DIRECTION('center_axis',(0.,0.,1.));
#4968=DIRECTION('ref_axis',(1.,0.,0.));
#4969=DIRECTION('axis',(0.,0.,1.));
#4970=DIRECTION('refdir',(1.,0.,0.));
#4971=DIRECTION('center_axis',(0.,1.,0.));
#4972=DIRECTION('ref_axis',(1.,0.,0.));
#4973=DIRECTION('center_axis',(0.,-1.,0.));
#4974=DIRECTION('ref_axis',(1.,0.,0.));
#4975=DIRECTION('',(0.,-1.,0.));
#4976=DIRECTION('center_axis',(0.,-1.,0.));
#4977=DIRECTION('ref_axis',(1.,0.,0.));
#4978=DIRECTION('center_axis',(0.,1.,0.));
#4979=DIRECTION('ref_axis',(1.,0.,0.));
#4980=DIRECTION('center_axis',(0.,1.,0.));
#4981=DIRECTION('ref_axis',(1.,0.,0.));
#4982=DIRECTION('',(0.,-1.,0.));
#4983=DIRECTION('center_axis',(0.,1.,0.));
#4984=DIRECTION('ref_axis',(1.,0.,0.));
#4985=DIRECTION('center_axis',(0.,1.,0.));
#4986=DIRECTION('ref_axis',(1.,0.,0.));
#4987=DIRECTION('center_axis',(0.,1.,0.));
#4988=DIRECTION('ref_axis',(1.,0.,0.));
#4989=DIRECTION('axis',(0.,0.,1.));
#4990=DIRECTION('refdir',(1.,0.,0.));
#4991=DIRECTION('center_axis',(0.,1.,0.));
#4992=DIRECTION('ref_axis',(1.,0.,0.));
#4993=DIRECTION('center_axis',(0.,1.,0.));
#4994=DIRECTION('ref_axis',(1.,0.,0.));
#4995=DIRECTION('',(0.,1.,0.));
#4996=DIRECTION('center_axis',(0.,-1.,0.));
#4997=DIRECTION('ref_axis',(1.,0.,0.));
#4998=DIRECTION('center_axis',(0.,1.,0.));
#4999=DIRECTION('ref_axis',(1.,0.,0.));
#5000=DIRECTION('center_axis',(0.,1.,0.));
#5001=DIRECTION('ref_axis',(1.,0.,0.));
#5002=DIRECTION('center_axis',(0.,1.,0.));
#5003=DIRECTION('ref_axis',(1.,0.,0.));
#5004=DIRECTION('center_axis',(0.,1.,0.));
#5005=DIRECTION('ref_axis',(1.,0.,0.));
#5006=DIRECTION('center_axis',(0.,1.,0.));
#5007=DIRECTION('ref_axis',(1.,0.,0.));
#5008=DIRECTION('',(0.,-1.,0.));
#5009=DIRECTION('center_axis',(0.,1.,0.));
#5010=DIRECTION('ref_axis',(1.,0.,0.));
#5011=DIRECTION('center_axis',(0.,1.,0.));
#5012=DIRECTION('ref_axis',(1.,0.,0.));
#5013=DIRECTION('center_axis',(0.,1.,0.));
#5014=DIRECTION('ref_axis',(1.,0.,0.));
#5015=DIRECTION('center_axis',(0.,1.,0.));
#5016=DIRECTION('ref_axis',(1.,0.,0.));
#5017=DIRECTION('',(0.,-1.,0.));
#5018=DIRECTION('center_axis',(0.,1.,0.));
#5019=DIRECTION('ref_axis',(1.,0.,0.));
#5020=DIRECTION('axis',(0.,0.,1.));
#5021=DIRECTION('refdir',(1.,0.,0.));
#5022=DIRECTION('center_axis',(0.,1.,0.));
#5023=DIRECTION('ref_axis',(1.,0.,0.));
#5024=DIRECTION('center_axis',(0.,-1.,0.));
#5025=DIRECTION('ref_axis',(1.,0.,0.));
#5026=DIRECTION('',(0.,-1.,0.));
#5027=DIRECTION('center_axis',(0.,-1.,0.));
#5028=DIRECTION('ref_axis',(1.,0.,0.));
#5029=DIRECTION('center_axis',(0.,1.,0.));
#5030=DIRECTION('ref_axis',(1.,0.,0.));
#5031=DIRECTION('center_axis',(0.,1.,0.));
#5032=DIRECTION('ref_axis',(1.,0.,0.));
#5033=DIRECTION('',(0.,-1.,0.));
#5034=DIRECTION('center_axis',(0.,1.,0.));
#5035=DIRECTION('ref_axis',(1.,0.,0.));
#5036=DIRECTION('center_axis',(0.,1.,0.));
#5037=DIRECTION('ref_axis',(1.,0.,0.));
#5038=DIRECTION('center_axis',(0.,1.,0.));
#5039=DIRECTION('ref_axis',(1.,0.,0.));
#5040=DIRECTION('axis',(0.,0.,1.));
#5041=DIRECTION('refdir',(1.,0.,0.));
#5042=DIRECTION('center_axis',(0.,1.,0.));
#5043=DIRECTION('ref_axis',(1.,0.,0.));
#5044=DIRECTION('center_axis',(0.,-1.,0.));
#5045=DIRECTION('ref_axis',(1.,0.,0.));
#5046=DIRECTION('',(0.,-1.,0.));
#5047=DIRECTION('center_axis',(0.,-1.,0.));
#5048=DIRECTION('ref_axis',(1.,0.,0.));
#5049=DIRECTION('center_axis',(0.,1.,0.));
#5050=DIRECTION('ref_axis',(1.,0.,0.));
#5051=DIRECTION('center_axis',(0.,1.,0.));
#5052=DIRECTION('ref_axis',(1.,0.,0.));
#5053=DIRECTION('',(0.,-1.,0.));
#5054=DIRECTION('center_axis',(0.,1.,0.));
#5055=DIRECTION('ref_axis',(1.,0.,0.));
#5056=DIRECTION('center_axis',(0.,1.,0.));
#5057=DIRECTION('ref_axis',(1.,0.,0.));
#5058=DIRECTION('center_axis',(0.,1.,0.));
#5059=DIRECTION('ref_axis',(1.,0.,0.));
#5060=DIRECTION('axis',(0.,0.,1.));
#5061=DIRECTION('refdir',(1.,0.,0.));
#5062=DIRECTION('center_axis',(0.,0.,1.));
#5063=DIRECTION('ref_axis',(1.,0.,0.));
#5064=DIRECTION('center_axis',(0.,0.,-1.));
#5065=DIRECTION('ref_axis',(1.,0.,0.));
#5066=DIRECTION('',(0.,0.,-1.));
#5067=DIRECTION('center_axis',(0.,0.,-1.));
#5068=DIRECTION('ref_axis',(1.,0.,0.));
#5069=DIRECTION('center_axis',(0.,0.,1.));
#5070=DIRECTION('ref_axis',(1.,0.,0.));
#5071=DIRECTION('center_axis',(0.,0.,1.));
#5072=DIRECTION('ref_axis',(1.,0.,0.));
#5073=DIRECTION('',(0.,0.,-1.));
#5074=DIRECTION('center_axis',(0.,0.,1.));
#5075=DIRECTION('ref_axis',(1.,0.,0.));
#5076=DIRECTION('center_axis',(0.,0.,1.));
#5077=DIRECTION('ref_axis',(1.,0.,0.));
#5078=DIRECTION('center_axis',(0.,0.,1.));
#5079=DIRECTION('ref_axis',(1.,0.,0.));
#5080=DIRECTION('axis',(0.,0.,1.));
#5081=DIRECTION('refdir',(1.,0.,0.));
#5082=DIRECTION('center_axis',(0.,1.,0.));
#5083=DIRECTION('ref_axis',(1.,0.,0.));
#5084=DIRECTION('center_axis',(0.,-1.,0.));
#5085=DIRECTION('ref_axis',(1.,0.,0.));
#5086=DIRECTION('',(0.,-1.,0.));
#5087=DIRECTION('center_axis',(0.,-1.,0.));
#5088=DIRECTION('ref_axis',(1.,0.,0.));
#5089=DIRECTION('center_axis',(0.,1.,0.));
#5090=DIRECTION('ref_axis',(1.,0.,0.));
#5091=DIRECTION('center_axis',(0.,1.,0.));
#5092=DIRECTION('ref_axis',(1.,0.,0.));
#5093=DIRECTION('',(0.,-1.,0.));
#5094=DIRECTION('center_axis',(0.,1.,0.));
#5095=DIRECTION('ref_axis',(1.,0.,0.));
#5096=DIRECTION('center_axis',(0.,1.,0.));
#5097=DIRECTION('ref_axis',(1.,0.,0.));
#5098=DIRECTION('center_axis',(0.,1.,0.));
#5099=DIRECTION('ref_axis',(1.,0.,0.));
#5100=DIRECTION('axis',(0.,0.,1.));
#5101=DIRECTION('refdir',(1.,0.,0.));
#5102=DIRECTION('center_axis',(0.866025403784439,0.,-0.5));
#5103=DIRECTION('ref_axis',(0.5,0.,0.866025403784439));
#5104=DIRECTION('',(-0.5,0.,-0.866025403784439));
#5105=DIRECTION('',(0.,-1.,0.));
#5106=DIRECTION('',(0.5,0.,0.866025403784439));
#5107=DIRECTION('',(0.,-1.,0.));
#5108=DIRECTION('center_axis',(1.60246890531964E-16,0.,-1.));
#5109=DIRECTION('ref_axis',(1.,0.,1.60246890531964E-16));
#5110=DIRECTION('',(-1.,0.,-1.60246890531964E-16));
#5111=DIRECTION('',(0.,-1.,0.));
#5112=DIRECTION('',(1.,0.,1.60246890531964E-16));
#5113=DIRECTION('center_axis',(-0.866025403784439,0.,-0.5));
#5114=DIRECTION('ref_axis',(0.5,0.,-0.866025403784439));
#5115=DIRECTION('',(-0.5,0.,0.866025403784439));
#5116=DIRECTION('',(0.,-1.,0.));
#5117=DIRECTION('',(0.5,0.,-0.866025403784439));
#5118=DIRECTION('center_axis',(-0.866025403784439,0.,0.5));
#5119=DIRECTION('ref_axis',(-0.5,0.,-0.866025403784439));
#5120=DIRECTION('',(0.5,0.,0.866025403784439));
#5121=DIRECTION('',(0.,-1.,0.));
#5122=DIRECTION('',(-0.5,0.,-0.866025403784439));
#5123=DIRECTION('center_axis',(-1.60246890531964E-16,0.,1.));
#5124=DIRECTION('ref_axis',(-1.,0.,-1.60246890531964E-16));
#5125=DIRECTION('',(1.,0.,1.60246890531964E-16));
#5126=DIRECTION('',(0.,-1.,0.));
#5127=DIRECTION('',(-1.,0.,-1.60246890531964E-16));
#5128=DIRECTION('center_axis',(0.866025403784439,0.,0.5));
#5129=DIRECTION('ref_axis',(-0.5,0.,0.866025403784439));
#5130=DIRECTION('',(0.5,0.,-0.866025403784439));
#5131=DIRECTION('',(-0.5,0.,0.866025403784439));
#5132=DIRECTION('center_axis',(0.,1.,0.));
#5133=DIRECTION('ref_axis',(1.,0.,0.));
#5134=DIRECTION('center_axis',(0.,-1.,0.));
#5135=DIRECTION('ref_axis',(0.,0.,-1.));
#5136=DIRECTION('center_axis',(0.,1.,0.));
#5137=DIRECTION('ref_axis',(1.,0.,0.));
#5138=DIRECTION('center_axis',(0.,1.,0.));
#5139=DIRECTION('ref_axis',(1.,0.,0.));
#5140=DIRECTION('center_axis',(0.,1.,0.));
#5141=DIRECTION('ref_axis',(1.,0.,0.));
#5142=DIRECTION('center_axis',(0.,1.,0.));
#5143=DIRECTION('ref_axis',(1.,0.,0.));
#5144=DIRECTION('',(0.,-1.,0.));
#5145=DIRECTION('center_axis',(0.,1.,0.));
#5146=DIRECTION('ref_axis',(1.,0.,0.));
#5147=DIRECTION('center_axis',(0.,1.,0.));
#5148=DIRECTION('ref_axis',(1.,0.,0.));
#5149=DIRECTION('center_axis',(0.,1.,0.));
#5150=DIRECTION('ref_axis',(0.,0.,1.));
#5151=DIRECTION('center_axis',(0.,-1.,0.));
#5152=DIRECTION('ref_axis',(1.,0.,0.));
#5153=DIRECTION('center_axis',(0.,-1.,0.));
#5154=DIRECTION('ref_axis',(1.,0.,0.));
#5155=DIRECTION('center_axis',(0.,-1.,0.));
#5156=DIRECTION('ref_axis',(1.,0.,0.));
#5157=DIRECTION('',(0.707106781186548,0.707106781186547,8.65956056235493E-17));
#5158=DIRECTION('center_axis',(0.,-1.,0.));
#5159=DIRECTION('ref_axis',(1.,0.,0.));
#5160=DIRECTION('center_axis',(0.,-1.,0.));
#5161=DIRECTION('ref_axis',(1.,0.,0.));
#5162=DIRECTION('',(0.,1.,0.));
#5163=DIRECTION('center_axis',(0.,1.,0.));
#5164=DIRECTION('ref_axis',(1.,0.,0.));
#5165=DIRECTION('center_axis',(0.,-1.,0.));
#5166=DIRECTION('ref_axis',(1.,0.,0.));
#5167=DIRECTION('',(-0.707106781186548,0.707106781186547,-8.65956056235494E-17));
#5168=DIRECTION('center_axis',(0.,-1.,0.));
#5169=DIRECTION('ref_axis',(0.,0.,-1.));
#5170=DIRECTION('center_axis',(0.,-1.,0.));
#5171=DIRECTION('ref_axis',(1.,0.,0.));
#5172=DIRECTION('center_axis',(0.,1.,0.));
#5173=DIRECTION('ref_axis',(1.,0.,0.));
#5174=DIRECTION('center_axis',(0.,1.,0.));
#5175=DIRECTION('ref_axis',(1.,0.,0.));
#5176=DIRECTION('',(-0.447213595499958,0.894427190999916,-5.47678698264203E-17));
#5177=DIRECTION('center_axis',(0.,-1.,0.));
#5178=DIRECTION('ref_axis',(1.,0.,0.));
#5179=DIRECTION('',(0.,1.,0.));
#5180=DIRECTION('axis',(0.,0.,1.));
#5181=DIRECTION('refdir',(1.,0.,0.));
#5182=DIRECTION('center_axis',(0.,1.,0.));
#5183=DIRECTION('ref_axis',(1.,0.,0.));
#5184=DIRECTION('center_axis',(0.,-1.,0.));
#5185=DIRECTION('ref_axis',(1.,0.,0.));
#5186=DIRECTION('',(0.,-1.,0.));
#5187=DIRECTION('center_axis',(0.,-1.,0.));
#5188=DIRECTION('ref_axis',(1.,0.,0.));
#5189=DIRECTION('center_axis',(0.,1.,0.));
#5190=DIRECTION('ref_axis',(1.,0.,0.));
#5191=DIRECTION('center_axis',(0.,1.,0.));
#5192=DIRECTION('ref_axis',(1.,0.,0.));
#5193=DIRECTION('',(0.,-1.,0.));
#5194=DIRECTION('center_axis',(0.,1.,0.));
#5195=DIRECTION('ref_axis',(1.,0.,0.));
#5196=DIRECTION('center_axis',(0.,1.,0.));
#5197=DIRECTION('ref_axis',(1.,0.,0.));
#5198=DIRECTION('center_axis',(0.,1.,0.));
#5199=DIRECTION('ref_axis',(1.,0.,0.));
#5200=DIRECTION('axis',(0.,0.,1.));
#5201=DIRECTION('refdir',(1.,0.,0.));
#5202=DIRECTION('center_axis',(0.,1.,0.));
#5203=DIRECTION('ref_axis',(1.,0.,0.));
#5204=DIRECTION('',(0.866025403784439,-0.5,1.06057523872491E-16));
#5205=DIRECTION('center_axis',(0.,-1.,0.));
#5206=DIRECTION('ref_axis',(1.,0.,0.));
#5207=DIRECTION('center_axis',(0.,-1.,0.));
#5208=DIRECTION('ref_axis',(1.,0.,0.));
#5209=DIRECTION('center_axis',(0.,1.,0.));
#5210=DIRECTION('ref_axis',(1.,0.,0.));
#5211=DIRECTION('',(-0.866025403784439,-0.5,-1.06057523872491E-16));
#5212=DIRECTION('center_axis',(1.4792020664489E-16,0.,-1.));
#5213=DIRECTION('ref_axis',(-1.,0.,-1.4792020664489E-16));
#5214=DIRECTION('',(0.,1.,0.));
#5215=DIRECTION('',(0.,1.,0.));
#5216=DIRECTION('center_axis',(-0.866025403784439,0.,-0.5));
#5217=DIRECTION('ref_axis',(-0.5,0.,0.866025403784439));
#5218=DIRECTION('',(0.,1.,0.));
#5219=DIRECTION('center_axis',(-0.866025403784439,0.,0.5));
#5220=DIRECTION('ref_axis',(0.5,0.,0.866025403784439));
#5221=DIRECTION('',(0.,1.,0.));
#5222=DIRECTION('center_axis',(0.,1.,0.));
#5223=DIRECTION('ref_axis',(1.,0.,0.));
#5224=DIRECTION('center_axis',(0.,1.,0.));
#5225=DIRECTION('ref_axis',(1.,0.,0.));
#5226=DIRECTION('',(0.,-1.,0.));
#5227=DIRECTION('center_axis',(0.,1.,0.));
#5228=DIRECTION('ref_axis',(1.,0.,0.));
#5229=DIRECTION('center_axis',(-2.95840413289779E-16,0.,1.));
#5230=DIRECTION('ref_axis',(1.,0.,2.95840413289779E-16));
#5231=DIRECTION('',(0.,1.,0.));
#5232=DIRECTION('center_axis',(0.866025403784439,0.,-0.5));
#5233=DIRECTION('ref_axis',(-0.5,0.,-0.866025403784439));
#5234=DIRECTION('',(0.,1.,0.));
#5235=DIRECTION('center_axis',(0.866025403784439,0.,0.5));
#5236=DIRECTION('ref_axis',(0.5,0.,-0.866025403784439));
#5237=DIRECTION('center_axis',(0.,1.,0.));
#5238=DIRECTION('ref_axis',(1.,0.,0.));
#5239=DIRECTION('center_axis',(0.,1.,0.));
#5240=DIRECTION('ref_axis',(1.,0.,0.));
#5241=DIRECTION('axis',(0.,0.,1.));
#5242=DIRECTION('refdir',(1.,0.,0.));
#5243=DIRECTION('center_axis',(0.,1.,0.));
#5244=DIRECTION('ref_axis',(0.,0.,1.));
#5245=DIRECTION('center_axis',(0.,-1.,0.));
#5246=DIRECTION('ref_axis',(1.,0.,0.));
#5247=DIRECTION('center_axis',(0.,-1.,0.));
#5248=DIRECTION('ref_axis',(1.,0.,0.));
#5249=DIRECTION('center_axis',(0.,-1.,0.));
#5250=DIRECTION('ref_axis',(1.,0.,0.));
#5251=DIRECTION('',(0.707106781186548,0.707106781186547,8.65956056235493E-17));
#5252=DIRECTION('center_axis',(0.,-1.,0.));
#5253=DIRECTION('ref_axis',(1.,0.,0.));
#5254=DIRECTION('center_axis',(0.,-1.,0.));
#5255=DIRECTION('ref_axis',(1.,0.,0.));
#5256=DIRECTION('',(0.,1.,0.));
#5257=DIRECTION('center_axis',(0.,1.,0.));
#5258=DIRECTION('ref_axis',(1.,0.,0.));
#5259=DIRECTION('center_axis',(0.,-1.,0.));
#5260=DIRECTION('ref_axis',(1.,0.,0.));
#5261=DIRECTION('',(-0.707106781186548,0.707106781186547,-8.65956056235494E-17));
#5262=DIRECTION('center_axis',(0.,-1.,0.));
#5263=DIRECTION('ref_axis',(0.,0.,-1.));
#5264=DIRECTION('center_axis',(0.,-1.,0.));
#5265=DIRECTION('ref_axis',(1.,0.,0.));
#5266=DIRECTION('center_axis',(0.,1.,0.));
#5267=DIRECTION('ref_axis',(1.,0.,0.));
#5268=DIRECTION('center_axis',(0.,1.,0.));
#5269=DIRECTION('ref_axis',(1.,0.,0.));
#5270=DIRECTION('',(-0.447213595499958,0.894427190999916,-5.47678698264203E-17));
#5271=DIRECTION('center_axis',(0.,-1.,0.));
#5272=DIRECTION('ref_axis',(1.,0.,0.));
#5273=DIRECTION('center_axis',(0.,1.,0.));
#5274=DIRECTION('ref_axis',(1.,0.,0.));
#5275=DIRECTION('',(0.,1.,0.));
#5276=DIRECTION('center_axis',(0.,1.,0.));
#5277=DIRECTION('ref_axis',(1.,0.,0.));
#5278=DIRECTION('center_axis',(0.,-1.,0.));
#5279=DIRECTION('ref_axis',(1.,0.,0.));
#5280=DIRECTION('',(-0.707106781186547,0.707106781186548,-8.65956056235493E-17));
#5281=DIRECTION('center_axis',(0.,-1.,0.));
#5282=DIRECTION('ref_axis',(0.,0.,-1.));
#5283=DIRECTION('center_axis',(0.866025403784439,0.,-0.5));
#5284=DIRECTION('ref_axis',(0.5,0.,0.866025403784439));
#5285=DIRECTION('',(-0.5,0.,-0.866025403784439));
#5286=DIRECTION('',(0.,-1.,0.));
#5287=DIRECTION('',(0.5,0.,0.866025403784439));
#5288=DIRECTION('',(0.,-1.,0.));
#5289=DIRECTION('center_axis',(1.60246890531964E-16,0.,-1.));
#5290=DIRECTION('ref_axis',(1.,0.,1.60246890531964E-16));
#5291=DIRECTION('',(-1.,0.,-1.60246890531964E-16));
#5292=DIRECTION('',(0.,-1.,0.));
#5293=DIRECTION('',(1.,0.,1.60246890531964E-16));
#5294=DIRECTION('center_axis',(-0.866025403784439,0.,-0.5));
#5295=DIRECTION('ref_axis',(0.5,0.,-0.866025403784439));
#5296=DIRECTION('',(-0.5,0.,0.866025403784439));
#5297=DIRECTION('',(0.,-1.,0.));
#5298=DIRECTION('',(0.5,0.,-0.866025403784439));
#5299=DIRECTION('center_axis',(-0.866025403784439,0.,0.5));
#5300=DIRECTION('ref_axis',(-0.5,0.,-0.866025403784439));
#5301=DIRECTION('',(0.5,0.,0.866025403784439));
#5302=DIRECTION('',(0.,-1.,0.));
#5303=DIRECTION('',(-0.5,0.,-0.866025403784439));
#5304=DIRECTION('center_axis',(-1.60246890531964E-16,0.,1.));
#5305=DIRECTION('ref_axis',(-1.,0.,-1.60246890531964E-16));
#5306=DIRECTION('',(1.,0.,1.60246890531964E-16));
#5307=DIRECTION('',(0.,-1.,0.));
#5308=DIRECTION('',(-1.,0.,-1.60246890531964E-16));
#5309=DIRECTION('center_axis',(0.866025403784439,0.,0.5));
#5310=DIRECTION('ref_axis',(-0.5,0.,0.866025403784439));
#5311=DIRECTION('',(0.5,0.,-0.866025403784439));
#5312=DIRECTION('',(-0.5,0.,0.866025403784439));
#5313=DIRECTION('center_axis',(0.,1.,0.));
#5314=DIRECTION('ref_axis',(1.,0.,0.));
#5315=DIRECTION('center_axis',(0.,-1.,0.));
#5316=DIRECTION('ref_axis',(0.,0.,-1.));
#5317=DIRECTION('',(0.,0.,1.));
#5318=DIRECTION('',(1.,0.,0.));
#5319=DIRECTION('',(0.,0.,1.));
#5320=DIRECTION('',(-1.,1.22464679914735E-16,0.));
#5321=DIRECTION('',(0.,0.,1.));
#5322=DIRECTION('',(1.,0.,0.));
#5323=DIRECTION('',(0.,0.,1.));
#5324=DIRECTION('',(1.,0.,0.));
#5325=DIRECTION('',(0.,0.,1.));
#5326=DIRECTION('',(1.,0.,0.));
#5327=DIRECTION('',(0.,0.,1.));
#5328=DIRECTION('',(1.,0.,0.));
#5329=DIRECTION('',(0.,0.,1.));
#5330=DIRECTION('',(1.,0.,0.));
#5331=DIRECTION('',(0.,0.,1.));
#5332=DIRECTION('',(1.,0.,0.));
#5333=DIRECTION('',(0.,0.,1.));
#5334=DIRECTION('',(1.,0.,0.));
#5335=DIRECTION('',(0.,0.,1.));
#5336=DIRECTION('',(1.,0.,0.));
#5337=DIRECTION('',(0.,0.,1.));
#5338=DIRECTION('',(1.,0.,0.));
#5339=DIRECTION('',(0.,0.,1.));
#5340=DIRECTION('',(1.,0.,0.));
#5341=DIRECTION('',(0.,0.,1.));
#5342=DIRECTION('',(1.,0.,0.));
#5343=DIRECTION('',(0.,0.,1.));
#5344=DIRECTION('',(1.,0.,0.));
#5345=DIRECTION('',(0.,0.,1.));
#5346=DIRECTION('',(1.,0.,0.));
#5347=DIRECTION('',(0.,0.,1.));
#5348=DIRECTION('',(1.,0.,0.));
#5349=DIRECTION('',(0.,0.,1.));
#5350=DIRECTION('',(1.,0.,0.));
#5351=DIRECTION('',(0.,0.,1.));
#5352=DIRECTION('',(1.,0.,0.));
#5353=DIRECTION('',(0.,0.,1.));
#5354=DIRECTION('',(1.,0.,0.));
#5355=DIRECTION('',(0.,0.,1.));
#5356=DIRECTION('',(1.,0.,0.));
#5357=DIRECTION('',(0.,0.,1.));
#5358=DIRECTION('',(1.,0.,0.));
#5359=DIRECTION('',(0.,0.,1.));
#5360=DIRECTION('',(1.,0.,0.));
#5361=DIRECTION('',(0.,0.,1.));
#5362=DIRECTION('',(1.,0.,0.));
#5363=DIRECTION('axis',(0.,0.,1.));
#5364=DIRECTION('refdir',(1.,0.,0.));
#5365=DIRECTION('axis',(0.,0.,1.));
#5366=DIRECTION('refdir',(1.,0.,0.));
#5367=DIRECTION('center_axis',(0.,1.,0.));
#5368=DIRECTION('ref_axis',(1.,0.,0.));
#5369=DIRECTION('center_axis',(0.,1.,0.));
#5370=DIRECTION('ref_axis',(1.,0.,0.));
#5371=DIRECTION('',(0.,1.,0.));
#5372=DIRECTION('center_axis',(0.,-1.,0.));
#5373=DIRECTION('ref_axis',(1.,0.,0.));
#5374=DIRECTION('center_axis',(0.,1.,0.));
#5375=DIRECTION('ref_axis',(1.,0.,0.));
#5376=DIRECTION('center_axis',(0.,1.,0.));
#5377=DIRECTION('ref_axis',(1.,0.,0.));
#5378=DIRECTION('',(0.,1.,0.));
#5379=DIRECTION('center_axis',(0.,-1.,0.));
#5380=DIRECTION('ref_axis',(1.,0.,0.));
#5381=DIRECTION('center_axis',(0.,1.,0.));
#5382=DIRECTION('ref_axis',(1.,0.,0.));
#5383=DIRECTION('center_axis',(0.,1.,0.));
#5384=DIRECTION('ref_axis',(1.,0.,0.));
#5385=DIRECTION('',(0.,1.,0.));
#5386=DIRECTION('center_axis',(0.,-1.,0.));
#5387=DIRECTION('ref_axis',(1.,0.,0.));
#5388=DIRECTION('center_axis',(0.,1.,0.));
#5389=DIRECTION('ref_axis',(1.,0.,0.));
#5390=DIRECTION('center_axis',(0.,1.,0.));
#5391=DIRECTION('ref_axis',(1.,0.,0.));
#5392=DIRECTION('',(0.,1.,0.));
#5393=DIRECTION('center_axis',(0.,-1.,0.));
#5394=DIRECTION('ref_axis',(1.,0.,0.));
#5395=DIRECTION('center_axis',(0.,-1.,0.));
#5396=DIRECTION('ref_axis',(1.,0.,0.));
#5397=DIRECTION('center_axis',(0.,-1.,0.));
#5398=DIRECTION('ref_axis',(1.,0.,0.));
#5399=DIRECTION('',(-0.707106781186547,-0.707106781186548,-8.65956056235493E-17));
#5400=DIRECTION('center_axis',(0.,-1.,0.));
#5401=DIRECTION('ref_axis',(1.,0.,0.));
#5402=DIRECTION('center_axis',(0.,1.,0.));
#5403=DIRECTION('ref_axis',(1.,0.,0.));
#5404=DIRECTION('center_axis',(0.,1.,0.));
#5405=DIRECTION('ref_axis',(1.,0.,0.));
#5406=DIRECTION('',(0.707106781186547,-0.707106781186548,8.65956056235493E-17));
#5407=DIRECTION('center_axis',(0.,1.,0.));
#5408=DIRECTION('ref_axis',(1.,0.,0.));
#5409=DIRECTION('center_axis',(0.,1.,0.));
#5410=DIRECTION('ref_axis',(1.,0.,0.));
#5411=DIRECTION('',(0.,-1.,0.));
#5412=DIRECTION('center_axis',(0.,1.,0.));
#5413=DIRECTION('ref_axis',(1.,0.,0.));
#5414=DIRECTION('center_axis',(0.,1.,0.));
#5415=DIRECTION('ref_axis',(1.,0.,0.));
#5416=DIRECTION('center_axis',(0.,1.,0.));
#5417=DIRECTION('ref_axis',(1.,0.,0.));
#5418=DIRECTION('center_axis',(0.,1.,0.));
#5419=DIRECTION('ref_axis',(1.,0.,0.));
#5420=DIRECTION('center_axis',(0.,-1.,0.));
#5421=DIRECTION('ref_axis',(1.,0.,0.));
#5422=DIRECTION('center_axis',(0.,1.,0.));
#5423=DIRECTION('ref_axis',(1.,0.,0.));
#5424=DIRECTION('',(0.,-1.,0.));
#5425=DIRECTION('center_axis',(0.,1.,0.));
#5426=DIRECTION('ref_axis',(1.,0.,0.));
#5427=DIRECTION('',(0.,-1.,0.));
#5428=DIRECTION('center_axis',(0.,1.,0.));
#5429=DIRECTION('ref_axis',(1.,0.,0.));
#5430=DIRECTION('center_axis',(0.,1.,0.));
#5431=DIRECTION('ref_axis',(1.,0.,0.));
#5432=DIRECTION('center_axis',(0.,-1.,0.));
#5433=DIRECTION('ref_axis',(1.,0.,0.));
#5434=DIRECTION('',(0.,-1.,0.));
#5435=DIRECTION('center_axis',(0.,-1.,0.));
#5436=DIRECTION('ref_axis',(1.,0.,0.));
#5437=DIRECTION('center_axis',(0.,1.,0.));
#5438=DIRECTION('ref_axis',(1.,0.,0.));
#5439=DIRECTION('center_axis',(0.,1.,0.));
#5440=DIRECTION('ref_axis',(1.,0.,0.));
#5441=DIRECTION('',(0.,-1.,0.));
#5442=DIRECTION('center_axis',(0.,1.,0.));
#5443=DIRECTION('ref_axis',(1.,0.,0.));
#5444=DIRECTION('center_axis',(0.,1.,0.));
#5445=DIRECTION('ref_axis',(1.,0.,0.));
#5446=DIRECTION('axis',(0.,0.,1.));
#5447=DIRECTION('refdir',(1.,0.,0.));
#5448=DIRECTION('center_axis',(0.,1.,0.));
#5449=DIRECTION('ref_axis',(1.,0.,0.));
#5450=DIRECTION('center_axis',(0.,-1.,0.));
#5451=DIRECTION('ref_axis',(1.,0.,0.));
#5452=DIRECTION('',(0.,-1.,0.));
#5453=DIRECTION('center_axis',(0.,-1.,0.));
#5454=DIRECTION('ref_axis',(1.,0.,0.));
#5455=DIRECTION('center_axis',(0.,1.,0.));
#5456=DIRECTION('ref_axis',(1.,0.,0.));
#5457=DIRECTION('center_axis',(0.,1.,0.));
#5458=DIRECTION('ref_axis',(1.,0.,0.));
#5459=DIRECTION('',(0.,-1.,0.));
#5460=DIRECTION('center_axis',(0.,1.,0.));
#5461=DIRECTION('ref_axis',(1.,0.,0.));
#5462=DIRECTION('center_axis',(0.,1.,0.));
#5463=DIRECTION('ref_axis',(1.,0.,0.));
#5464=DIRECTION('center_axis',(0.,1.,0.));
#5465=DIRECTION('ref_axis',(1.,0.,0.));
#5466=DIRECTION('axis',(0.,0.,1.));
#5467=DIRECTION('refdir',(1.,0.,0.));
#5468=DIRECTION('axis',(0.,0.,1.));
#5469=DIRECTION('refdir',(1.,0.,0.));
#5470=DIRECTION('center_axis',(0.,-1.,0.));
#5471=DIRECTION('ref_axis',(0.,0.,-1.));
#5472=DIRECTION('center_axis',(0.,-1.,0.));
#5473=DIRECTION('ref_axis',(1.,0.,0.));
#5474=DIRECTION('center_axis',(0.,-1.,0.));
#5475=DIRECTION('ref_axis',(1.,0.,0.));
#5476=DIRECTION('center_axis',(1.,0.,1.22464679914735E-16));
#5477=DIRECTION('ref_axis',(-1.22464679914735E-16,0.,1.));
#5478=DIRECTION('center_axis',(0.,1.,0.));
#5479=DIRECTION('ref_axis',(1.,0.,0.));
#5480=DIRECTION('center_axis',(0.,1.,0.));
#5481=DIRECTION('ref_axis',(1.,0.,0.));
#5482=DIRECTION('center_axis',(0.,-1.,0.));
#5483=DIRECTION('ref_axis',(1.,0.,0.));
#5484=DIRECTION('',(0.,1.,0.));
#5485=DIRECTION('center_axis',(0.,-1.,0.));
#5486=DIRECTION('ref_axis',(1.,0.,0.));
#5487=DIRECTION('center_axis',(0.,-1.,0.));
#5488=DIRECTION('ref_axis',(1.,0.,0.));
#5489=DIRECTION('center_axis',(0.,-1.,0.));
#5490=DIRECTION('ref_axis',(1.,0.,0.));
#5491=DIRECTION('',(0.,1.,0.));
#5492=DIRECTION('center_axis',(0.,-1.,0.));
#5493=DIRECTION('ref_axis',(1.,0.,0.));
#5494=DIRECTION('center_axis',(0.,1.,0.));
#5495=DIRECTION('ref_axis',(1.,0.,0.));
#5496=DIRECTION('',(-0.707106781186548,0.707106781186547,-8.65956056235494E-17));
#5497=DIRECTION('center_axis',(0.,-1.,0.));
#5498=DIRECTION('ref_axis',(1.,0.,0.));
#5499=DIRECTION('center_axis',(0.,1.,0.));
#5500=DIRECTION('ref_axis',(0.,0.,1.));
#5501=DIRECTION('center_axis',(0.,-1.,0.));
#5502=DIRECTION('ref_axis',(1.,0.,0.));
#5503=DIRECTION('center_axis',(0.,-1.,0.));
#5504=DIRECTION('ref_axis',(1.,0.,0.));
#5505=DIRECTION('',(0.,1.,0.));
#5506=DIRECTION('center_axis',(0.,-1.,0.));
#5507=DIRECTION('ref_axis',(0.,0.,-1.));
#5508=DIRECTION('center_axis',(0.,-1.,0.));
#5509=DIRECTION('ref_axis',(1.,0.,0.));
#5510=DIRECTION('center_axis',(0.,-1.,0.));
#5511=DIRECTION('ref_axis',(1.,0.,0.));
#5512=DIRECTION('',(0.707106781186548,0.707106781186547,8.65956056235494E-17));
#5513=DIRECTION('axis',(0.,0.,1.));
#5514=DIRECTION('refdir',(1.,0.,0.));
#5515=DIRECTION('center_axis',(0.,-1.,0.));
#5516=DIRECTION('ref_axis',(0.,0.,-1.));
#5517=DIRECTION('center_axis',(0.,-1.,0.));
#5518=DIRECTION('ref_axis',(1.,0.,0.));
#5519=DIRECTION('center_axis',(0.,-1.,0.));
#5520=DIRECTION('ref_axis',(1.,0.,0.));
#5521=DIRECTION('center_axis',(1.,0.,1.22464679914735E-16));
#5522=DIRECTION('ref_axis',(-1.22464679914735E-16,0.,1.));
#5523=DIRECTION('center_axis',(0.,1.,0.));
#5524=DIRECTION('ref_axis',(1.,0.,0.));
#5525=DIRECTION('center_axis',(0.,1.,0.));
#5526=DIRECTION('ref_axis',(1.,0.,0.));
#5527=DIRECTION('center_axis',(0.,-1.,0.));
#5528=DIRECTION('ref_axis',(1.,0.,0.));
#5529=DIRECTION('center_axis',(0.,-1.,0.));
#5530=DIRECTION('ref_axis',(1.,0.,0.));
#5531=DIRECTION('',(0.,1.,0.));
#5532=DIRECTION('center_axis',(0.,1.,0.));
#5533=DIRECTION('ref_axis',(0.,0.,1.));
#5534=DIRECTION('center_axis',(0.,-1.,0.));
#5535=DIRECTION('ref_axis',(1.,0.,0.));
#5536=DIRECTION('center_axis',(0.,-1.,0.));
#5537=DIRECTION('ref_axis',(1.,0.,0.));
#5538=DIRECTION('center_axis',(0.,-1.,0.));
#5539=DIRECTION('ref_axis',(1.,0.,0.));
#5540=DIRECTION('center_axis',(0.,-1.,0.));
#5541=DIRECTION('ref_axis',(1.,0.,0.));
#5542=DIRECTION('',(0.707106781186548,0.707106781186547,8.65956056235494E-17));
#5543=DIRECTION('center_axis',(0.,-1.,0.));
#5544=DIRECTION('ref_axis',(1.,0.,0.));
#5545=DIRECTION('center_axis',(0.,-1.,0.));
#5546=DIRECTION('ref_axis',(1.,0.,0.));
#5547=DIRECTION('',(0.,1.,0.));
#5548=DIRECTION('center_axis',(0.,1.,0.));
#5549=DIRECTION('ref_axis',(1.,0.,0.));
#5550=DIRECTION('center_axis',(0.,-1.,0.));
#5551=DIRECTION('ref_axis',(1.,0.,0.));
#5552=DIRECTION('',(-0.707106781186548,0.707106781186547,-8.65956056235494E-17));
#5553=DIRECTION('center_axis',(0.,-1.,0.));
#5554=DIRECTION('ref_axis',(0.,0.,-1.));
#5555=DIRECTION('center_axis',(0.,-1.,0.));
#5556=DIRECTION('ref_axis',(1.,0.,0.));
#5557=DIRECTION('',(0.,1.,0.));
#5558=DIRECTION('axis',(0.,0.,1.));
#5559=DIRECTION('refdir',(1.,0.,0.));
#5560=DIRECTION('center_axis',(0.,0.,1.));
#5561=DIRECTION('ref_axis',(1.,0.,0.));
#5562=DIRECTION('center_axis',(1.22464679914735E-16,-1.,0.));
#5563=DIRECTION('ref_axis',(-1.,-1.22464679914735E-16,0.));
#5564=DIRECTION('center_axis',(0.707106781186548,0.,0.707106781186548));
#5565=DIRECTION('ref_axis',(0.707106781186548,0.,-0.707106781186548));
#5566=DIRECTION('center_axis',(8.65956056235493E-17,-1.,-8.65956056235493E-17));
#5567=DIRECTION('ref_axis',(-0.707106781186548,-1.22464679914735E-16,0.707106781186548));
#5568=DIRECTION('center_axis',(1.,0.,0.));
#5569=DIRECTION('ref_axis',(6.12323399573677E-17,0.,-1.));
#5570=DIRECTION('center_axis',(7.49879891330929E-33,-1.,-1.22464679914735E-16));
#5571=DIRECTION('ref_axis',(-6.12323399573677E-17,-1.22464679914735E-16,
1.));
#5572=DIRECTION('center_axis',(0.707106781186548,0.,-0.707106781186548));
#5573=DIRECTION('ref_axis',(-0.707106781186548,0.,-0.707106781186548));
#5574=DIRECTION('center_axis',(-8.65956056235493E-17,-1.,-8.65956056235493E-17));
#5575=DIRECTION('ref_axis',(0.707106781186548,-1.22464679914735E-16,0.707106781186548));
#5576=DIRECTION('center_axis',(0.,0.,-1.));
#5577=DIRECTION('ref_axis',(-1.,0.,-1.22464679914735E-16));
#5578=DIRECTION('center_axis',(-1.22464679914735E-16,-1.,-1.49975978266186E-32));
#5579=DIRECTION('ref_axis',(1.,-1.22464679914735E-16,1.22464679914735E-16));
#5580=DIRECTION('center_axis',(-0.707106781186548,0.,-0.707106781186548));
#5581=DIRECTION('ref_axis',(-0.707106781186548,0.,0.707106781186548));
#5582=DIRECTION('center_axis',(-8.65956056235493E-17,-1.,8.65956056235493E-17));
#5583=DIRECTION('ref_axis',(0.707106781186548,-1.22464679914735E-16,-0.707106781186548));
#5584=DIRECTION('center_axis',(-1.,0.,0.));
#5585=DIRECTION('ref_axis',(-1.83697019872103E-16,0.,1.));
#5586=DIRECTION('center_axis',(-2.24963967399279E-32,-1.,1.22464679914735E-16));
#5587=DIRECTION('ref_axis',(1.83697019872103E-16,-1.22464679914735E-16,
-1.));
#5588=DIRECTION('center_axis',(-0.707106781186548,0.,0.707106781186548));
#5589=DIRECTION('ref_axis',(0.707106781186548,0.,0.707106781186548));
#5590=DIRECTION('center_axis',(8.65956056235493E-17,-1.,8.65956056235494E-17));
#5591=DIRECTION('ref_axis',(-0.707106781186548,-1.22464679914735E-16,-0.707106781186548));
#5592=DIRECTION('axis',(0.,0.,1.));
#5593=DIRECTION('refdir',(1.,0.,0.));
#5594=DIRECTION('center_axis',(0.,0.,1.));
#5595=DIRECTION('ref_axis',(1.,0.,0.));
#5596=DIRECTION('center_axis',(0.,-1.,0.));
#5597=DIRECTION('ref_axis',(0.,0.,-1.));
#5598=DIRECTION('center_axis',(0.,-1.,0.));
#5599=DIRECTION('ref_axis',(0.,0.,-1.));
#5600=DIRECTION('center_axis',(0.,1.,0.));
#5601=DIRECTION('ref_axis',(1.,0.,0.));
#5602=DIRECTION('center_axis',(0.,1.,0.));
#5603=DIRECTION('ref_axis',(1.,0.,0.));
#5604=DIRECTION('center_axis',(0.,1.,0.));
#5605=DIRECTION('ref_axis',(1.,0.,0.));
#5606=DIRECTION('center_axis',(0.,1.,0.));
#5607=DIRECTION('ref_axis',(1.,0.,0.));
#5608=DIRECTION('',(0.,-1.,0.));
#5609=DIRECTION('center_axis',(0.,-1.,0.));
#5610=DIRECTION('ref_axis',(1.,0.,0.));
#5611=DIRECTION('center_axis',(0.,1.,0.));
#5612=DIRECTION('ref_axis',(1.,0.,0.));
#5613=DIRECTION('center_axis',(0.,1.,0.));
#5614=DIRECTION('ref_axis',(1.,0.,0.));
#5615=DIRECTION('center_axis',(0.,1.,0.));
#5616=DIRECTION('ref_axis',(1.,0.,0.));
#5617=DIRECTION('center_axis',(0.,1.,0.));
#5618=DIRECTION('ref_axis',(1.,0.,0.));
#5619=DIRECTION('center_axis',(0.,1.,0.));
#5620=DIRECTION('ref_axis',(1.,0.,0.));
#5621=DIRECTION('center_axis',(0.,1.,0.));
#5622=DIRECTION('ref_axis',(1.,0.,0.));
#5623=DIRECTION('center_axis',(0.,-1.,0.));
#5624=DIRECTION('ref_axis',(1.,0.,0.));
#5625=DIRECTION('center_axis',(0.,-1.,0.));
#5626=DIRECTION('ref_axis',(0.,0.,-1.));
#5627=DIRECTION('center_axis',(6.12323399573677E-17,0.,1.));
#5628=DIRECTION('ref_axis',(1.,0.,0.));
#5629=DIRECTION('center_axis',(0.,-1.,0.));
#5630=DIRECTION('ref_axis',(0.,0.,-1.));
#5631=DIRECTION('center_axis',(0.,1.,0.));
#5632=DIRECTION('ref_axis',(1.,0.,0.));
#5633=DIRECTION('center_axis',(0.,-1.,0.));
#5634=DIRECTION('ref_axis',(1.,0.,0.));
#5635=DIRECTION('center_axis',(0.,-1.,0.));
#5636=DIRECTION('ref_axis',(0.,0.,-1.));
#5637=DIRECTION('center_axis',(0.,0.,1.));
#5638=DIRECTION('ref_axis',(1.,0.,0.));
#5639=DIRECTION('center_axis',(0.,-1.,0.));
#5640=DIRECTION('ref_axis',(0.,0.,-1.));
#5641=DIRECTION('center_axis',(0.,1.,0.));
#5642=DIRECTION('ref_axis',(1.,0.,0.));
#5643=DIRECTION('center_axis',(0.,-1.,0.));
#5644=DIRECTION('ref_axis',(1.,0.,0.));
#5645=DIRECTION('center_axis',(0.,-1.,0.));
#5646=DIRECTION('ref_axis',(0.,0.,-1.));
#5647=DIRECTION('center_axis',(0.,0.,1.));
#5648=DIRECTION('ref_axis',(1.,0.,0.));
#5649=DIRECTION('center_axis',(0.,-1.,0.));
#5650=DIRECTION('ref_axis',(0.,0.,-1.));
#5651=DIRECTION('center_axis',(0.,1.,0.));
#5652=DIRECTION('ref_axis',(1.,0.,0.));
#5653=DIRECTION('center_axis',(0.,-1.,0.));
#5654=DIRECTION('ref_axis',(1.,0.,0.));
#5655=DIRECTION('center_axis',(0.,-1.,0.));
#5656=DIRECTION('ref_axis',(0.,0.,-1.));
#5657=DIRECTION('center_axis',(0.,0.,1.));
#5658=DIRECTION('ref_axis',(1.,0.,0.));
#5659=DIRECTION('center_axis',(0.,-1.,0.));
#5660=DIRECTION('ref_axis',(0.,0.,-1.));
#5661=DIRECTION('center_axis',(0.,1.,0.));
#5662=DIRECTION('ref_axis',(1.,0.,0.));
#5663=DIRECTION('center_axis',(0.,-1.,0.));
#5664=DIRECTION('ref_axis',(1.,0.,0.));
#5665=DIRECTION('center_axis',(0.,-1.,0.));
#5666=DIRECTION('ref_axis',(0.,0.,-1.));
#5667=DIRECTION('center_axis',(6.12323399573676E-17,0.,1.));
#5668=DIRECTION('ref_axis',(1.,0.,0.));
#5669=DIRECTION('center_axis',(0.,-1.,0.));
#5670=DIRECTION('ref_axis',(0.,0.,-1.));
#5671=DIRECTION('center_axis',(0.,1.,0.));
#5672=DIRECTION('ref_axis',(1.,0.,0.));
#5673=DIRECTION('center_axis',(0.,-1.,0.));
#5674=DIRECTION('ref_axis',(1.,0.,0.));
#5675=DIRECTION('center_axis',(0.,-1.,0.));
#5676=DIRECTION('ref_axis',(0.,0.,-1.));
#5677=DIRECTION('center_axis',(0.,0.,1.));
#5678=DIRECTION('ref_axis',(1.,0.,0.));
#5679=DIRECTION('center_axis',(0.,-1.,0.));
#5680=DIRECTION('ref_axis',(0.,0.,-1.));
#5681=DIRECTION('center_axis',(0.,1.,0.));
#5682=DIRECTION('ref_axis',(1.,0.,0.));
#5683=DIRECTION('center_axis',(0.,1.,0.));
#5684=DIRECTION('ref_axis',(1.,0.,0.));
#5685=DIRECTION('',(0.,1.,0.));
#5686=DIRECTION('center_axis',(0.,-1.,0.));
#5687=DIRECTION('ref_axis',(1.,0.,0.));
#5688=DIRECTION('center_axis',(0.,-1.,0.));
#5689=DIRECTION('ref_axis',(1.,0.,0.));
#5690=DIRECTION('center_axis',(0.,1.,0.));
#5691=DIRECTION('ref_axis',(1.,0.,0.));
#5692=DIRECTION('center_axis',(0.,-1.,0.));
#5693=DIRECTION('ref_axis',(0.,0.,-1.));
#5694=DIRECTION('center_axis',(0.,0.,1.));
#5695=DIRECTION('ref_axis',(1.,0.,0.));
#5696=DIRECTION('center_axis',(0.,-1.,0.));
#5697=DIRECTION('ref_axis',(0.,0.,-1.));
#5698=DIRECTION('center_axis',(0.,-1.,0.));
#5699=DIRECTION('ref_axis',(-1.,0.,0.));
#5700=DIRECTION('center_axis',(0.,1.,0.));
#5701=DIRECTION('ref_axis',(1.,0.,0.));
#5702=DIRECTION('axis',(0.,0.,1.));
#5703=DIRECTION('refdir',(1.,0.,0.));
#5704=DIRECTION('center_axis',(0.,1.,0.));
#5705=DIRECTION('ref_axis',(0.,0.,1.));
#5706=DIRECTION('center_axis',(0.,-1.,0.));
#5707=DIRECTION('ref_axis',(1.,0.,0.));
#5708=DIRECTION('center_axis',(0.,-1.,0.));
#5709=DIRECTION('ref_axis',(1.,0.,0.));
#5710=DIRECTION('center_axis',(0.,-1.,0.));
#5711=DIRECTION('ref_axis',(1.,0.,0.));
#5712=DIRECTION('center_axis',(0.,-1.,0.));
#5713=DIRECTION('ref_axis',(1.,0.,0.));
#5714=DIRECTION('',(0.,1.,0.));
#5715=DIRECTION('center_axis',(0.,-1.,0.));
#5716=DIRECTION('ref_axis',(0.,0.,-1.));
#5717=DIRECTION('center_axis',(0.,-1.,0.));
#5718=DIRECTION('ref_axis',(1.,0.,0.));
#5719=DIRECTION('center_axis',(0.,-1.,0.));
#5720=DIRECTION('ref_axis',(1.,0.,0.));
#5721=DIRECTION('',(0.,1.,0.));
#5722=DIRECTION('center_axis',(0.,1.,0.));
#5723=DIRECTION('ref_axis',(0.,0.,1.));
#5724=DIRECTION('center_axis',(0.,-1.,0.));
#5725=DIRECTION('ref_axis',(1.,0.,0.));
#5726=DIRECTION('center_axis',(0.,-1.,0.));
#5727=DIRECTION('ref_axis',(1.,0.,0.));
#5728=DIRECTION('center_axis',(0.,-1.,0.));
#5729=DIRECTION('ref_axis',(1.,0.,0.));
#5730=DIRECTION('center_axis',(0.,-1.,0.));
#5731=DIRECTION('ref_axis',(1.,0.,0.));
#5732=DIRECTION('',(0.,1.,0.));
#5733=DIRECTION('center_axis',(0.,-1.,0.));
#5734=DIRECTION('ref_axis',(0.,0.,-1.));
#5735=DIRECTION('center_axis',(0.,-1.,0.));
#5736=DIRECTION('ref_axis',(1.,0.,0.));
#5737=DIRECTION('center_axis',(0.,-1.,0.));
#5738=DIRECTION('ref_axis',(1.,0.,0.));
#5739=DIRECTION('',(0.,1.,0.));
#5740=DIRECTION('',(0.,0.,1.));
#5741=DIRECTION('',(1.,0.,0.));
#5742=DIRECTION('',(0.,0.,1.));
#5743=DIRECTION('',(1.,0.,0.));
#5744=DIRECTION('',(0.,0.,1.));
#5745=DIRECTION('',(1.,0.,0.));
#5746=DIRECTION('',(0.,0.,1.));
#5747=DIRECTION('',(1.,0.,0.));
#5748=DIRECTION('',(0.,0.,1.));
#5749=DIRECTION('',(1.,0.,0.));
#5750=DIRECTION('axis',(0.,0.,1.));
#5751=DIRECTION('refdir',(1.,0.,0.));
#5752=DIRECTION('center_axis',(0.,1.,0.));
#5753=DIRECTION('ref_axis',(1.,0.,0.));
#5754=DIRECTION('center_axis',(0.,1.,0.));
#5755=DIRECTION('ref_axis',(1.,0.,0.));
#5756=DIRECTION('',(0.,1.,0.));
#5757=DIRECTION('center_axis',(0.,-1.,0.));
#5758=DIRECTION('ref_axis',(1.,0.,0.));
#5759=DIRECTION('center_axis',(0.,1.,0.));
#5760=DIRECTION('ref_axis',(1.,0.,0.));
#5761=DIRECTION('center_axis',(0.,1.,0.));
#5762=DIRECTION('ref_axis',(1.,0.,0.));
#5763=DIRECTION('',(0.,1.,0.));
#5764=DIRECTION('center_axis',(0.,-1.,0.));
#5765=DIRECTION('ref_axis',(1.,0.,0.));
#5766=DIRECTION('center_axis',(0.,1.,0.));
#5767=DIRECTION('ref_axis',(1.,0.,0.));
#5768=DIRECTION('center_axis',(0.,1.,0.));
#5769=DIRECTION('ref_axis',(1.,0.,0.));
#5770=DIRECTION('',(0.,1.,0.));
#5771=DIRECTION('center_axis',(0.,-1.,0.));
#5772=DIRECTION('ref_axis',(1.,0.,0.));
#5773=DIRECTION('center_axis',(0.,1.,0.));
#5774=DIRECTION('ref_axis',(1.,0.,0.));
#5775=DIRECTION('center_axis',(0.,1.,0.));
#5776=DIRECTION('ref_axis',(1.,0.,0.));
#5777=DIRECTION('',(0.,1.,0.));
#5778=DIRECTION('center_axis',(0.,-1.,0.));
#5779=DIRECTION('ref_axis',(1.,0.,0.));
#5780=DIRECTION('center_axis',(0.,1.,0.));
#5781=DIRECTION('ref_axis',(1.,0.,0.));
#5782=DIRECTION('center_axis',(0.,1.,0.));
#5783=DIRECTION('ref_axis',(1.,0.,0.));
#5784=DIRECTION('',(0.,-1.,0.));
#5785=DIRECTION('center_axis',(0.,-1.,0.));
#5786=DIRECTION('ref_axis',(1.,0.,0.));
#5787=DIRECTION('center_axis',(0.,1.,0.));
#5788=DIRECTION('ref_axis',(1.,0.,0.));
#5789=DIRECTION('center_axis',(0.,-1.,0.));
#5790=DIRECTION('ref_axis',(1.,0.,0.));
#5791=DIRECTION('center_axis',(0.,1.,0.));
#5792=DIRECTION('ref_axis',(1.,0.,0.));
#5793=DIRECTION('',(0.,-1.,0.));
#5794=DIRECTION('center_axis',(0.,-1.,0.));
#5795=DIRECTION('ref_axis',(1.,0.,0.));
#5796=DIRECTION('center_axis',(0.,1.,0.));
#5797=DIRECTION('ref_axis',(1.,0.,0.));
#5798=DIRECTION('center_axis',(0.,1.,0.));
#5799=DIRECTION('ref_axis',(1.,0.,0.));
#5800=DIRECTION('',(0.,-1.,0.));
#5801=DIRECTION('center_axis',(0.,1.,0.));
#5802=DIRECTION('ref_axis',(1.,0.,0.));
#5803=DIRECTION('center_axis',(0.,1.,0.));
#5804=DIRECTION('ref_axis',(1.,0.,0.));
#5805=DIRECTION('center_axis',(0.,1.,0.));
#5806=DIRECTION('ref_axis',(1.,0.,0.));
#5807=DIRECTION('axis',(0.,0.,1.));
#5808=DIRECTION('refdir',(1.,0.,0.));
#5809=DIRECTION('center_axis',(0.866025403784439,0.,-0.5));
#5810=DIRECTION('ref_axis',(0.5,0.,0.866025403784439));
#5811=DIRECTION('',(-0.5,0.,-0.866025403784439));
#5812=DIRECTION('',(0.,-1.,0.));
#5813=DIRECTION('',(0.5,0.,0.866025403784439));
#5814=DIRECTION('',(0.,-1.,0.));
#5815=DIRECTION('center_axis',(1.60246890531964E-16,0.,-1.));
#5816=DIRECTION('ref_axis',(1.,0.,1.60246890531964E-16));
#5817=DIRECTION('',(-1.,0.,-1.60246890531964E-16));
#5818=DIRECTION('',(0.,-1.,0.));
#5819=DIRECTION('',(1.,0.,1.60246890531964E-16));
#5820=DIRECTION('center_axis',(-0.866025403784439,0.,-0.5));
#5821=DIRECTION('ref_axis',(0.5,0.,-0.866025403784439));
#5822=DIRECTION('',(-0.5,0.,0.866025403784439));
#5823=DIRECTION('',(0.,-1.,0.));
#5824=DIRECTION('',(0.5,0.,-0.866025403784439));
#5825=DIRECTION('center_axis',(-0.866025403784439,0.,0.5));
#5826=DIRECTION('ref_axis',(-0.5,0.,-0.866025403784439));
#5827=DIRECTION('',(0.5,0.,0.866025403784439));
#5828=DIRECTION('',(0.,-1.,0.));
#5829=DIRECTION('',(-0.5,0.,-0.866025403784439));
#5830=DIRECTION('center_axis',(-1.60246890531964E-16,0.,1.));
#5831=DIRECTION('ref_axis',(-1.,0.,-1.60246890531964E-16));
#5832=DIRECTION('',(1.,0.,1.60246890531964E-16));
#5833=DIRECTION('',(0.,-1.,0.));
#5834=DIRECTION('',(-1.,0.,-1.60246890531964E-16));
#5835=DIRECTION('center_axis',(0.866025403784439,0.,0.5));
#5836=DIRECTION('ref_axis',(-0.5,0.,0.866025403784439));
#5837=DIRECTION('',(0.5,0.,-0.866025403784439));
#5838=DIRECTION('',(-0.5,0.,0.866025403784439));
#5839=DIRECTION('center_axis',(0.,1.,0.));
#5840=DIRECTION('ref_axis',(1.,0.,0.));
#5841=DIRECTION('center_axis',(0.,-1.,0.));
#5842=DIRECTION('ref_axis',(0.,0.,-1.));
#5843=DIRECTION('center_axis',(0.,1.,0.));
#5844=DIRECTION('ref_axis',(1.,0.,0.));
#5845=DIRECTION('center_axis',(0.,1.,0.));
#5846=DIRECTION('ref_axis',(1.,0.,0.));
#5847=DIRECTION('center_axis',(0.,1.,0.));
#5848=DIRECTION('ref_axis',(0.,0.,1.));
#5849=DIRECTION('center_axis',(0.,-1.,0.));
#5850=DIRECTION('ref_axis',(1.,0.,0.));
#5851=DIRECTION('center_axis',(0.,-1.,0.));
#5852=DIRECTION('ref_axis',(1.,0.,0.));
#5853=DIRECTION('center_axis',(0.,-1.,0.));
#5854=DIRECTION('ref_axis',(1.,0.,0.));
#5855=DIRECTION('',(0.707106781186547,0.707106781186548,8.65956056235493E-17));
#5856=DIRECTION('center_axis',(0.,-1.,0.));
#5857=DIRECTION('ref_axis',(1.,0.,0.));
#5858=DIRECTION('center_axis',(0.,-1.,0.));
#5859=DIRECTION('ref_axis',(1.,0.,0.));
#5860=DIRECTION('',(0.,1.,0.));
#5861=DIRECTION('center_axis',(0.,1.,0.));
#5862=DIRECTION('ref_axis',(1.,0.,0.));
#5863=DIRECTION('center_axis',(0.,-1.,0.));
#5864=DIRECTION('ref_axis',(1.,0.,0.));
#5865=DIRECTION('',(-0.707106781186547,0.707106781186548,-8.65956056235493E-17));
#5866=DIRECTION('center_axis',(0.,-1.,0.));
#5867=DIRECTION('ref_axis',(0.,0.,-1.));
#5868=DIRECTION('center_axis',(0.,-1.,0.));
#5869=DIRECTION('ref_axis',(1.,0.,0.));
#5870=DIRECTION('center_axis',(0.,1.,0.));
#5871=DIRECTION('ref_axis',(1.,0.,0.));
#5872=DIRECTION('center_axis',(0.,1.,0.));
#5873=DIRECTION('ref_axis',(1.,0.,0.));
#5874=DIRECTION('',(-0.447213595499958,0.894427190999916,-5.47678698264203E-17));
#5875=DIRECTION('center_axis',(0.,-1.,0.));
#5876=DIRECTION('ref_axis',(1.,0.,0.));
#5877=DIRECTION('',(0.,1.,0.));
#5878=DIRECTION('',(0.,0.,1.));
#5879=DIRECTION('',(1.,0.,0.));
#5880=DIRECTION('',(0.,0.,1.));
#5881=DIRECTION('',(1.,0.,0.));
#5882=DIRECTION('',(0.,0.,1.));
#5883=DIRECTION('',(1.,0.,0.));
#5884=DIRECTION('',(0.,0.,1.));
#5885=DIRECTION('',(1.,0.,0.));
#5886=DIRECTION('',(0.,0.,1.));
#5887=DIRECTION('',(1.,0.,0.));
#5888=DIRECTION('',(0.,0.,1.));
#5889=DIRECTION('',(-1.,1.22464679914735E-16,0.));
#5890=DIRECTION('',(0.,0.,1.));
#5891=DIRECTION('',(-1.,1.22464679914735E-16,0.));
#5892=DIRECTION('',(0.,0.,1.));
#5893=DIRECTION('',(-1.,1.22464679914735E-16,0.));
#5894=DIRECTION('',(0.,0.,1.));
#5895=DIRECTION('',(-1.,1.22464679914735E-16,0.));
#5896=DIRECTION('',(0.,0.,1.));
#5897=DIRECTION('',(-1.,1.22464679914735E-16,0.));
#5898=DIRECTION('',(0.,0.,1.));
#5899=DIRECTION('',(1.,0.,0.));
#5900=DIRECTION('',(0.,0.,1.));
#5901=DIRECTION('',(1.,0.,0.));
#5902=DIRECTION('',(0.,0.,1.));
#5903=DIRECTION('',(1.,0.,0.));
#5904=DIRECTION('',(0.,0.,1.));
#5905=DIRECTION('',(1.,0.,0.));
#5906=DIRECTION('axis',(0.,0.,1.));
#5907=DIRECTION('refdir',(1.,0.,0.));
#5908=DIRECTION('axis',(0.,0.,1.));
#5909=DIRECTION('refdir',(1.,0.,0.));
#5910=DIRECTION('center_axis',(0.,0.,1.));
#5911=DIRECTION('ref_axis',(1.,0.,0.));
#5912=DIRECTION('center_axis',(0.,0.,1.));
#5913=DIRECTION('ref_axis',(1.,0.,0.));
#5914=DIRECTION('center_axis',(0.,0.,1.));
#5915=DIRECTION('ref_axis',(1.,0.,0.));
#5916=DIRECTION('center_axis',(0.,0.,1.));
#5917=DIRECTION('ref_axis',(1.,0.,0.));
#5918=DIRECTION('center_axis',(0.,0.,1.));
#5919=DIRECTION('ref_axis',(1.,0.,0.));
#5920=DIRECTION('center_axis',(0.,0.,-1.));
#5921=DIRECTION('ref_axis',(1.,0.,0.));
#5922=DIRECTION('center_axis',(0.,0.,1.));
#5923=DIRECTION('ref_axis',(1.,0.,0.));
#5924=DIRECTION('',(0.,0.,-1.));
#5925=DIRECTION('center_axis',(0.,0.,1.));
#5926=DIRECTION('ref_axis',(1.,0.,0.));
#5927=DIRECTION('',(0.,0.,-1.));
#5928=DIRECTION('center_axis',(0.,0.,-1.));
#5929=DIRECTION('ref_axis',(1.,0.,0.));
#5930=DIRECTION('center_axis',(0.,0.,-1.));
#5931=DIRECTION('ref_axis',(1.,0.,0.));
#5932=DIRECTION('center_axis',(0.,0.,-1.));
#5933=DIRECTION('ref_axis',(1.,0.,0.));
#5934=DIRECTION('center_axis',(0.,0.,1.));
#5935=DIRECTION('ref_axis',(1.,0.,0.));
#5936=DIRECTION('center_axis',(0.,0.,1.));
#5937=DIRECTION('ref_axis',(1.,0.,0.));
#5938=DIRECTION('',(0.,0.,-1.));
#5939=DIRECTION('center_axis',(0.,0.,1.));
#5940=DIRECTION('ref_axis',(1.,0.,0.));
#5941=DIRECTION('center_axis',(0.,0.,1.));
#5942=DIRECTION('ref_axis',(1.,0.,0.));
#5943=DIRECTION('',(-1.,0.,0.));
#5944=DIRECTION('',(0.,1.,0.));
#5945=DIRECTION('',(1.,0.,0.));
#5946=DIRECTION('center_axis',(0.,0.,1.));
#5947=DIRECTION('ref_axis',(1.,0.,0.));
#5948=DIRECTION('',(1.,0.,0.));
#5949=DIRECTION('',(0.,1.,0.));
#5950=DIRECTION('',(-1.,0.,0.));
#5951=DIRECTION('center_axis',(-1.,0.,0.));
#5952=DIRECTION('ref_axis',(0.,0.,1.));
#5953=DIRECTION('',(0.,1.,0.));
#5954=DIRECTION('',(0.,0.,-1.));
#5955=DIRECTION('',(0.,0.,1.));
#5956=DIRECTION('center_axis',(0.,0.,-1.));
#5957=DIRECTION('ref_axis',(-1.,0.,0.));
#5958=DIRECTION('',(0.,-1.,0.));
#5959=DIRECTION('',(-1.,0.,0.));
#5960=DIRECTION('',(0.,1.,0.));
#5961=DIRECTION('',(1.,0.,0.));
#5962=DIRECTION('center_axis',(0.,1.,0.));
#5963=DIRECTION('ref_axis',(1.,0.,0.));
#5964=DIRECTION('',(0.,0.,-1.));
#5965=DIRECTION('center_axis',(0.,-1.,0.));
#5966=DIRECTION('ref_axis',(1.,0.,0.));
#5967=DIRECTION('',(1.,0.,0.));
#5968=DIRECTION('center_axis',(0.,1.,0.));
#5969=DIRECTION('ref_axis',(1.,0.,0.));
#5970=DIRECTION('center_axis',(0.,1.,0.));
#5971=DIRECTION('ref_axis',(1.,0.,0.));
#5972=DIRECTION('center_axis',(0.,-1.,0.));
#5973=DIRECTION('ref_axis',(1.,0.,0.));
#5974=DIRECTION('',(0.,1.,0.));
#5975=DIRECTION('center_axis',(0.,1.,0.));
#5976=DIRECTION('ref_axis',(1.,0.,0.));
#5977=DIRECTION('',(0.,0.,1.));
#5978=DIRECTION('center_axis',(0.,1.,0.));
#5979=DIRECTION('ref_axis',(1.,0.,0.));
#5980=DIRECTION('',(-1.,0.,0.));
#5981=DIRECTION('center_axis',(-1.,0.,0.));
#5982=DIRECTION('ref_axis',(0.,0.,1.));
#5983=DIRECTION('center_axis',(0.,0.,-1.));
#5984=DIRECTION('ref_axis',(-1.,0.,0.));
#5985=DIRECTION('',(0.,-1.,0.));
#5986=DIRECTION('center_axis',(0.,1.,0.));
#5987=DIRECTION('ref_axis',(-0.267261241912424,0.,-0.963624111659432));
#5988=DIRECTION('axis',(0.,0.,1.));
#5989=DIRECTION('refdir',(1.,0.,0.));
#5990=DIRECTION('center_axis',(0.,0.,1.));
#5991=DIRECTION('ref_axis',(1.,0.,0.));
#5992=DIRECTION('center_axis',(0.,0.,-1.));
#5993=DIRECTION('ref_axis',(1.,0.,0.));
#5994=DIRECTION('',(0.,0.,-1.));
#5995=DIRECTION('center_axis',(0.,0.,-1.));
#5996=DIRECTION('ref_axis',(1.,0.,0.));
#5997=DIRECTION('center_axis',(0.,0.,1.));
#5998=DIRECTION('ref_axis',(1.,0.,0.));
#5999=DIRECTION('center_axis',(0.,0.,1.));
#6000=DIRECTION('ref_axis',(1.,0.,0.));
#6001=DIRECTION('',(0.,0.,-1.));
#6002=DIRECTION('center_axis',(0.,0.,1.));
#6003=DIRECTION('ref_axis',(1.,0.,0.));
#6004=DIRECTION('center_axis',(0.,0.,1.));
#6005=DIRECTION('ref_axis',(1.,0.,0.));
#6006=DIRECTION('center_axis',(0.,0.,1.));
#6007=DIRECTION('ref_axis',(1.,0.,0.));
#6008=DIRECTION('axis',(0.,0.,1.));
#6009=DIRECTION('refdir',(1.,0.,0.));
#6010=DIRECTION('center_axis',(0.,0.,1.));
#6011=DIRECTION('ref_axis',(1.,0.,0.));
#6012=DIRECTION('center_axis',(0.,0.,1.));
#6013=DIRECTION('ref_axis',(1.,0.,0.));
#6014=DIRECTION('',(0.,0.,1.));
#6015=DIRECTION('center_axis',(0.,0.,-1.));
#6016=DIRECTION('ref_axis',(1.,0.,0.));
#6017=DIRECTION('center_axis',(-1.60246890531964E-16,-1.,0.));
#6018=DIRECTION('ref_axis',(1.,-1.60246890531964E-16,0.));
#6019=DIRECTION('',(1.,-1.60246890531964E-16,0.));
#6020=DIRECTION('',(0.,0.,1.));
#6021=DIRECTION('',(1.,-1.60246890531964E-16,0.));
#6022=DIRECTION('',(0.,0.,1.));
#6023=DIRECTION('center_axis',(-0.866025403784439,-0.5,0.));
#6024=DIRECTION('ref_axis',(0.5,-0.866025403784439,0.));
#6025=DIRECTION('',(0.5,-0.866025403784439,0.));
#6026=DIRECTION('',(0.5,-0.866025403784439,0.));
#6027=DIRECTION('',(0.,0.,1.));
#6028=DIRECTION('center_axis',(-0.866025403784439,0.5,0.));
#6029=DIRECTION('ref_axis',(-0.5,-0.866025403784439,0.));
#6030=DIRECTION('',(-0.5,-0.866025403784439,0.));
#6031=DIRECTION('',(-0.5,-0.866025403784439,0.));
#6032=DIRECTION('',(0.,0.,1.));
#6033=DIRECTION('center_axis',(1.60246890531964E-16,1.,0.));
#6034=DIRECTION('ref_axis',(-1.,1.60246890531964E-16,0.));
#6035=DIRECTION('',(-1.,1.60246890531964E-16,0.));
#6036=DIRECTION('',(-1.,1.60246890531964E-16,0.));
#6037=DIRECTION('',(0.,0.,1.));
#6038=DIRECTION('center_axis',(0.866025403784439,0.5,0.));
#6039=DIRECTION('ref_axis',(-0.5,0.866025403784439,0.));
#6040=DIRECTION('',(-0.5,0.866025403784439,0.));
#6041=DIRECTION('',(-0.5,0.866025403784439,0.));
#6042=DIRECTION('',(0.,0.,1.));
#6043=DIRECTION('center_axis',(0.866025403784439,-0.5,0.));
#6044=DIRECTION('ref_axis',(0.5,0.866025403784439,0.));
#6045=DIRECTION('',(0.5,0.866025403784439,0.));
#6046=DIRECTION('',(0.5,0.866025403784439,0.));
#6047=DIRECTION('center_axis',(0.,0.,1.));
#6048=DIRECTION('ref_axis',(1.,0.,0.));
#6049=DIRECTION('center_axis',(0.,0.,1.));
#6050=DIRECTION('ref_axis',(1.,0.,0.));
#6051=DIRECTION('',(0.,0.,1.));
#6052=DIRECTION('',(1.,0.,0.));
#6053=DIRECTION('',(0.,0.,1.));
#6054=DIRECTION('',(1.,0.,0.));
#6055=DIRECTION('',(0.,0.,1.));
#6056=DIRECTION('',(1.,0.,0.));
#6057=DIRECTION('',(0.,0.,1.));
#6058=DIRECTION('',(1.,0.,0.));
#6059=DIRECTION('',(0.,0.,1.));
#6060=DIRECTION('',(1.,0.,0.));
#6061=DIRECTION('',(0.,0.,1.));
#6062=DIRECTION('',(1.,0.,0.));
#6063=CARTESIAN_POINT('',(0.,0.,0.));
#6064=CARTESIAN_POINT('',(0.,0.,0.));
#6065=CARTESIAN_POINT('',(0.,0.,0.));
#6066=CARTESIAN_POINT('Origin',(0.,-2.8,12.));
#6067=CARTESIAN_POINT('',(-2.99903459153175,-2.8,10.7476855351806));
#6068=CARTESIAN_POINT('',(-2.60150387000671,-2.8,10.0520067725117));
#6069=CARTESIAN_POINT('Origin',(-3.5,-2.8,10.));
#6070=CARTESIAN_POINT('',(-2.99903459153175,-2.8,13.2523144648194));
#6071=CARTESIAN_POINT('Origin',(0.,-2.8,12.));
#6072=CARTESIAN_POINT('',(-2.60150387000671,-2.8,13.9479932274883));
#6073=CARTESIAN_POINT('Origin',(-3.5,-2.8,14.));
#6074=CARTESIAN_POINT('',(2.60150387000671,-2.8,13.9479932274883));
#6075=CARTESIAN_POINT('Origin',(0.,-2.8,12.));
#6076=CARTESIAN_POINT('',(2.99903459153175,-2.8,13.2523144648194));
#6077=CARTESIAN_POINT('Origin',(3.5,-2.8,14.));
#6078=CARTESIAN_POINT('',(2.99903459153175,-2.8,10.7476855351806));
#6079=CARTESIAN_POINT('Origin',(0.,-2.8,12.));
#6080=CARTESIAN_POINT('',(2.60150387000671,-2.8,10.0520067725117));
#6081=CARTESIAN_POINT('Origin',(3.5,-2.8,10.));
#6082=CARTESIAN_POINT('Origin',(0.,-2.8,12.));
#6083=CARTESIAN_POINT('',(-1.2,-2.8,12.));
#6084=CARTESIAN_POINT('Origin',(0.,-2.8,12.));
#6085=CARTESIAN_POINT('Origin',(0.,-2.8,12.));
#6086=CARTESIAN_POINT('',(2.99903459153175,-2.5,10.7476855351806));
#6087=CARTESIAN_POINT('',(2.99903459153175,-2.8,10.7476855351806));
#6088=CARTESIAN_POINT('',(2.99903459153175,-2.5,13.2523144648194));
#6089=CARTESIAN_POINT('',(2.99903459153175,-2.8,13.2523144648194));
#6090=CARTESIAN_POINT('Origin',(0.,-2.5,12.));
#6091=CARTESIAN_POINT('Origin',(0.,-2.8,12.));
#6092=CARTESIAN_POINT('',(-2.60150387000671,-2.5,13.9479932274883));
#6093=CARTESIAN_POINT('',(-2.60150387000671,-2.8,13.9479932274883));
#6094=CARTESIAN_POINT('',(2.60150387000671,-2.5,13.9479932274883));
#6095=CARTESIAN_POINT('Origin',(0.,-2.5,12.));
#6096=CARTESIAN_POINT('',(2.60150387000671,-2.8,13.9479932274883));
#6097=CARTESIAN_POINT('Origin',(0.,-2.8,12.));
#6098=CARTESIAN_POINT('',(-2.60150387000671,-2.5,10.0520067725117));
#6099=CARTESIAN_POINT('',(-2.60150387000671,-2.8,10.0520067725117));
#6100=CARTESIAN_POINT('',(2.60150387000671,-2.5,10.0520067725117));
#6101=CARTESIAN_POINT('',(2.60150387000671,-2.8,10.0520067725117));
#6102=CARTESIAN_POINT('Origin',(0.,-2.5,12.));
#6103=CARTESIAN_POINT('Origin',(0.,-2.8,12.));
#6104=CARTESIAN_POINT('',(-1.2,-2.5,12.));
#6105=CARTESIAN_POINT('',(-1.2,-2.8,12.));
#6106=CARTESIAN_POINT('Origin',(0.,-2.5,12.));
#6107=CARTESIAN_POINT('Origin',(0.,-2.8,12.));
#6108=CARTESIAN_POINT('',(-2.99903459153175,-2.5,10.7476855351806));
#6109=CARTESIAN_POINT('',(-2.99903459153175,-2.8,10.7476855351806));
#6110=CARTESIAN_POINT('',(-2.99903459153175,-2.5,13.2523144648194));
#6111=CARTESIAN_POINT('Origin',(0.,-2.5,12.));
#6112=CARTESIAN_POINT('',(-2.99903459153175,-2.8,13.2523144648194));
#6113=CARTESIAN_POINT('Origin',(-3.5,-3.2,10.));
#6114=CARTESIAN_POINT('',(-4.4,-3.1,10.));
#6115=CARTESIAN_POINT('Origin',(-3.5,-3.1,10.));
#6116=CARTESIAN_POINT('',(-4.4,-2.5,10.));
#6117=CARTESIAN_POINT('',(-4.4,-3.2,10.));
#6118=CARTESIAN_POINT('Origin',(-3.5,-2.5,10.));
#6119=CARTESIAN_POINT('Origin',(-3.5,-2.5,10.));
#6120=CARTESIAN_POINT('Origin',(3.5,-3.2,10.));
#6121=CARTESIAN_POINT('',(2.6,-3.1,10.));
#6122=CARTESIAN_POINT('Origin',(3.5,-3.1,10.));
#6123=CARTESIAN_POINT('',(2.6,-2.5,10.));
#6124=CARTESIAN_POINT('',(2.6,-3.2,10.));
#6125=CARTESIAN_POINT('Origin',(3.5,-2.5,10.));
#6126=CARTESIAN_POINT('Origin',(3.5,-2.5,10.));
#6127=CARTESIAN_POINT('Origin',(3.5,-3.2,14.));
#6128=CARTESIAN_POINT('',(2.6,-3.1,14.));
#6129=CARTESIAN_POINT('Origin',(3.5,-3.1,14.));
#6130=CARTESIAN_POINT('',(2.6,-2.5,14.));
#6131=CARTESIAN_POINT('',(2.6,-3.2,14.));
#6132=CARTESIAN_POINT('Origin',(3.5,-2.5,14.));
#6133=CARTESIAN_POINT('Origin',(3.5,-2.5,14.));
#6134=CARTESIAN_POINT('Origin',(0.,-2.5,13.25));
#6135=CARTESIAN_POINT('',(-1.,-2.5,12.));
#6136=CARTESIAN_POINT('Origin',(0.,-2.5,12.));
#6137=CARTESIAN_POINT('Origin',(-3.5,-3.2,14.));
#6138=CARTESIAN_POINT('',(-4.4,-3.1,14.));
#6139=CARTESIAN_POINT('Origin',(-3.5,-3.1,14.));
#6140=CARTESIAN_POINT('',(-4.4,-2.5,14.));
#6141=CARTESIAN_POINT('',(-4.4,-3.2,14.));
#6142=CARTESIAN_POINT('Origin',(-3.5,-2.5,14.));
#6143=CARTESIAN_POINT('Origin',(-3.5,-2.5,14.));
#6144=CARTESIAN_POINT('Origin',(-2.,-3.2,5.));
#6145=CARTESIAN_POINT('',(-2.425,-3.1,5.));
#6146=CARTESIAN_POINT('Origin',(-2.,-3.1,5.));
#6147=CARTESIAN_POINT('',(-2.425,-2.5,5.));
#6148=CARTESIAN_POINT('',(-2.425,-3.2,5.));
#6149=CARTESIAN_POINT('Origin',(-2.,-2.5,5.));
#6150=CARTESIAN_POINT('Origin',(2.,-3.2,5.));
#6151=CARTESIAN_POINT('',(1.575,-3.1,5.));
#6152=CARTESIAN_POINT('Origin',(2.,-3.1,5.));
#6153=CARTESIAN_POINT('',(1.575,-2.5,5.));
#6154=CARTESIAN_POINT('',(1.575,-3.2,5.));
#6155=CARTESIAN_POINT('Origin',(2.,-2.5,5.));
#6156=CARTESIAN_POINT('Origin',(0.,-3.2,20.5));
#6157=CARTESIAN_POINT('',(-0.425,-3.1,20.5));
#6158=CARTESIAN_POINT('Origin',(0.,-3.1,20.5));
#6159=CARTESIAN_POINT('',(-0.425,-2.5,20.5));
#6160=CARTESIAN_POINT('',(-0.425,-3.2,20.5));
#6161=CARTESIAN_POINT('Origin',(0.,-2.5,20.5));
#6162=CARTESIAN_POINT('Origin',(0.,-3.2,12.));
#6163=CARTESIAN_POINT('',(-1.,-3.1,12.));
#6164=CARTESIAN_POINT('Origin',(0.,-3.1,12.));
#6165=CARTESIAN_POINT('',(-1.,-3.2,12.));
#6166=CARTESIAN_POINT('Origin',(-3.,-3.1,4.5));
#6167=CARTESIAN_POINT('',(-6.,-3.1,9.));
#6168=CARTESIAN_POINT('',(-3.,-3.1,4.5));
#6169=CARTESIAN_POINT('',(-6.,-3.1,9.));
#6170=CARTESIAN_POINT('',(-6.,-2.5,9.));
#6171=CARTESIAN_POINT('',(-6.,-3.1,9.));
#6172=CARTESIAN_POINT('',(-3.,-2.5,4.5));
#6173=CARTESIAN_POINT('',(-6.,-2.5,9.));
#6174=CARTESIAN_POINT('',(-3.,-3.1,4.5));
#6175=CARTESIAN_POINT('Origin',(3.,-3.1,4.5));
#6176=CARTESIAN_POINT('',(3.,-3.1,4.5));
#6177=CARTESIAN_POINT('',(-3.,-3.1,4.5));
#6178=CARTESIAN_POINT('',(3.,-2.5,4.5));
#6179=CARTESIAN_POINT('',(-3.,-2.5,4.5));
#6180=CARTESIAN_POINT('',(3.,-3.1,4.5));
#6181=CARTESIAN_POINT('Origin',(6.,-3.1,9.));
#6182=CARTESIAN_POINT('',(6.,-3.1,9.));
#6183=CARTESIAN_POINT('',(3.,-3.1,4.5));
#6184=CARTESIAN_POINT('',(6.,-2.5,9.));
#6185=CARTESIAN_POINT('',(3.,-2.5,4.5));
#6186=CARTESIAN_POINT('',(6.,-3.1,9.));
#6187=CARTESIAN_POINT('Origin',(6.,-3.1,15.));
#6188=CARTESIAN_POINT('',(6.,-3.1,15.));
#6189=CARTESIAN_POINT('',(6.,-3.1,9.));
#6190=CARTESIAN_POINT('',(6.,-2.5,15.));
#6191=CARTESIAN_POINT('',(6.,-2.5,9.));
#6192=CARTESIAN_POINT('',(6.,-3.1,15.));
#6193=CARTESIAN_POINT('Origin',(2.5,-3.1,22.));
#6194=CARTESIAN_POINT('',(2.5,-3.1,22.));
#6195=CARTESIAN_POINT('',(6.,-3.1,15.));
#6196=CARTESIAN_POINT('',(2.5,-2.5,22.));
#6197=CARTESIAN_POINT('',(6.,-2.5,15.));
#6198=CARTESIAN_POINT('',(2.5,-3.1,22.));
#6199=CARTESIAN_POINT('Origin',(-2.5,-3.1,22.));
#6200=CARTESIAN_POINT('',(-2.5,-3.1,22.));
#6201=CARTESIAN_POINT('',(2.5,-3.1,22.));
#6202=CARTESIAN_POINT('',(-2.5,-2.5,22.));
#6203=CARTESIAN_POINT('',(2.5,-2.5,22.));
#6204=CARTESIAN_POINT('',(-2.5,-3.1,22.));
#6205=CARTESIAN_POINT('Origin',(-6.,-3.1,15.));
#6206=CARTESIAN_POINT('',(-6.,-3.1,15.));
#6207=CARTESIAN_POINT('',(-2.5,-3.1,22.));
#6208=CARTESIAN_POINT('',(-6.,-2.5,15.));
#6209=CARTESIAN_POINT('',(-2.5,-2.5,22.));
#6210=CARTESIAN_POINT('',(-6.,-3.1,15.));
#6211=CARTESIAN_POINT('Origin',(-6.,-3.1,9.));
#6212=CARTESIAN_POINT('',(-6.,-3.1,15.));
#6213=CARTESIAN_POINT('',(-6.,-2.5,15.));
#6214=CARTESIAN_POINT('Origin',(0.,-2.5,13.25));
#6215=CARTESIAN_POINT('Origin',(0.,-3.1,13.25));
#6216=CARTESIAN_POINT('',(0.,0.,0.));
#6217=CARTESIAN_POINT('Origin',(0.,0.,4.4));
#6218=CARTESIAN_POINT('',(-1.1,-1.34711147906209E-16,4.5));
#6219=CARTESIAN_POINT('Origin',(0.,0.,4.5));
#6220=CARTESIAN_POINT('',(-1.1,1.34711147906209E-16,5.5));
#6221=CARTESIAN_POINT('',(-1.1,-1.34711147906209E-16,4.4));
#6222=CARTESIAN_POINT('Origin',(0.,0.,5.5));
#6223=CARTESIAN_POINT('Origin',(-2.,-2.6,5.));
#6224=CARTESIAN_POINT('',(-2.425,-2.5,5.));
#6225=CARTESIAN_POINT('Origin',(-2.,-2.5,5.));
#6226=CARTESIAN_POINT('',(-2.425,2.5,5.));
#6227=CARTESIAN_POINT('',(-2.425,-2.6,5.));
#6228=CARTESIAN_POINT('Origin',(-2.,2.5,5.));
#6229=CARTESIAN_POINT('Origin',(2.,-2.6,5.));
#6230=CARTESIAN_POINT('',(1.575,-2.5,5.));
#6231=CARTESIAN_POINT('Origin',(2.,-2.5,5.));
#6232=CARTESIAN_POINT('',(1.575,2.5,5.));
#6233=CARTESIAN_POINT('',(1.575,-2.6,5.));
#6234=CARTESIAN_POINT('Origin',(2.,2.5,5.));
#6235=CARTESIAN_POINT('Origin',(3.,2.5,4.5));
#6236=CARTESIAN_POINT('',(3.,2.5,4.5));
#6237=CARTESIAN_POINT('',(-3.,2.5,4.5));
#6238=CARTESIAN_POINT('',(3.,2.5,4.5));
#6239=CARTESIAN_POINT('',(-3.,2.5,5.5));
#6240=CARTESIAN_POINT('',(-3.,2.5,4.5));
#6241=CARTESIAN_POINT('',(3.,2.5,5.5));
#6242=CARTESIAN_POINT('',(3.,2.5,5.5));
#6243=CARTESIAN_POINT('',(3.,2.5,4.5));
#6244=CARTESIAN_POINT('Origin',(3.,-2.5,4.5));
#6245=CARTESIAN_POINT('',(3.,-2.5,4.5));
#6246=CARTESIAN_POINT('',(3.,-2.5,4.5));
#6247=CARTESIAN_POINT('',(3.,-2.5,5.5));
#6248=CARTESIAN_POINT('',(3.,-2.5,5.5));
#6249=CARTESIAN_POINT('',(3.,-2.5,4.5));
#6250=CARTESIAN_POINT('Origin',(-3.,-2.5,4.5));
#6251=CARTESIAN_POINT('',(-3.,-2.5,4.5));
#6252=CARTESIAN_POINT('',(-3.,-2.5,4.5));
#6253=CARTESIAN_POINT('',(-3.,-2.5,5.5));
#6254=CARTESIAN_POINT('',(-3.,-2.5,5.5));
#6255=CARTESIAN_POINT('',(-3.,-2.5,4.5));
#6256=CARTESIAN_POINT('Origin',(-3.,2.5,4.5));
#6257=CARTESIAN_POINT('',(-3.,2.5,4.5));
#6258=CARTESIAN_POINT('',(-3.,2.5,5.5));
#6259=CARTESIAN_POINT('Origin',(0.,0.,5.5));
#6260=CARTESIAN_POINT('Origin',(0.,0.,4.5));
#6261=CARTESIAN_POINT('',(0.,0.,0.));
#6262=CARTESIAN_POINT('Origin',(0.,-2.5,20.5));
#6263=CARTESIAN_POINT('',(-0.425,2.5,20.5));
#6264=CARTESIAN_POINT('Origin',(0.,2.5,20.5));
#6265=CARTESIAN_POINT('',(-0.425,-2.5,20.5));
#6266=CARTESIAN_POINT('',(-0.425,-2.5,20.5));
#6267=CARTESIAN_POINT('Origin',(0.,-2.5,20.5));
#6268=CARTESIAN_POINT('Origin',(0.,-2.5,20.5));
#6269=CARTESIAN_POINT('',(-1.,2.5,20.5));
#6270=CARTESIAN_POINT('Origin',(0.,2.5,20.5));
#6271=CARTESIAN_POINT('',(-1.,-2.5,20.5));
#6272=CARTESIAN_POINT('',(-1.,-2.5,20.5));
#6273=CARTESIAN_POINT('Origin',(0.,-2.5,20.5));
#6274=CARTESIAN_POINT('Origin',(0.,2.5,20.5));
#6275=CARTESIAN_POINT('Origin',(0.,-2.5,20.5));
#6276=CARTESIAN_POINT('',(0.,0.,0.));
#6277=CARTESIAN_POINT('Origin',(0.,0.3,12.));
#6278=CARTESIAN_POINT('',(-0.34,0.3,12.));
#6279=CARTESIAN_POINT('Origin',(0.,0.3,12.));
#6280=CARTESIAN_POINT('',(-0.34,3.1,12.));
#6281=CARTESIAN_POINT('',(-0.34,0.3,12.));
#6282=CARTESIAN_POINT('Origin',(0.,3.1,12.));
#6283=CARTESIAN_POINT('Origin',(0.,0.3,12.));
#6284=CARTESIAN_POINT('Origin',(0.,-3.1,12.));
#6285=CARTESIAN_POINT('',(-1.5,-3.1,12.));
#6286=CARTESIAN_POINT('Origin',(0.,-3.1,12.));
#6287=CARTESIAN_POINT('',(-1.,-3.1,12.));
#6288=CARTESIAN_POINT('Origin',(0.,-3.1,12.));
#6289=CARTESIAN_POINT('Origin',(0.,-3.5,12.));
#6290=CARTESIAN_POINT('',(-1.5,-3.5,12.));
#6291=CARTESIAN_POINT('',(-1.5,-3.5,12.));
#6292=CARTESIAN_POINT('Origin',(0.,-3.5,12.));
#6293=CARTESIAN_POINT('Origin',(0.,-3.5,12.));
#6294=CARTESIAN_POINT('Origin',(0.,-3.1,12.));
#6295=CARTESIAN_POINT('',(-1.,3.1,12.));
#6296=CARTESIAN_POINT('Origin',(0.,3.1,12.));
#6297=CARTESIAN_POINT('',(-1.,-3.1,12.));
#6298=CARTESIAN_POINT('Origin',(0.,3.1,12.));
#6299=CARTESIAN_POINT('',(0.,0.,0.));
#6300=CARTESIAN_POINT('Origin',(0.,3.1,12.));
#6301=CARTESIAN_POINT('',(-0.425,3.4,12.));
#6302=CARTESIAN_POINT('Origin',(0.,3.4,12.));
#6303=CARTESIAN_POINT('',(-0.425,3.1,12.));
#6304=CARTESIAN_POINT('',(-0.425,3.1,12.));
#6305=CARTESIAN_POINT('Origin',(0.,3.1,12.));
#6306=CARTESIAN_POINT('Origin',(0.,3.1,12.));
#6307=CARTESIAN_POINT('',(-1.5,3.4,12.));
#6308=CARTESIAN_POINT('Origin',(0.,3.4,12.));
#6309=CARTESIAN_POINT('',(-1.5,3.1,12.));
#6310=CARTESIAN_POINT('',(-1.5,3.1,12.));
#6311=CARTESIAN_POINT('Origin',(0.,3.1,12.));
#6312=CARTESIAN_POINT('Origin',(0.,3.4,12.));
#6313=CARTESIAN_POINT('Origin',(0.,3.1,12.));
#6314=CARTESIAN_POINT('',(0.,0.,0.));
#6315=CARTESIAN_POINT('Origin',(0.,-0.3,12.));
#6316=CARTESIAN_POINT('',(-1.005,0.3,12.));
#6317=CARTESIAN_POINT('Origin',(0.,0.3,12.));
#6318=CARTESIAN_POINT('',(-1.005,-0.3,12.));
#6319=CARTESIAN_POINT('',(-1.005,-0.3,12.));
#6320=CARTESIAN_POINT('Origin',(0.,-0.3,12.));
#6321=CARTESIAN_POINT('Origin',(0.,-0.3,12.));
#6322=CARTESIAN_POINT('',(-1.4,0.3,12.));
#6323=CARTESIAN_POINT('Origin',(0.,0.3,12.));
#6324=CARTESIAN_POINT('',(-1.4,-0.3,12.));
#6325=CARTESIAN_POINT('',(-1.4,-0.3,12.));
#6326=CARTESIAN_POINT('Origin',(0.,-0.3,12.));
#6327=CARTESIAN_POINT('Origin',(0.,0.3,12.));
#6328=CARTESIAN_POINT('Origin',(0.,-0.3,12.));
#6329=CARTESIAN_POINT('',(0.,0.,0.));
#6330=CARTESIAN_POINT('Origin',(0.,0.,4.5));
#6331=CARTESIAN_POINT('',(-0.81,-9.91963907309356E-17,5.5));
#6332=CARTESIAN_POINT('Origin',(0.,0.,5.5));
#6333=CARTESIAN_POINT('',(-0.81,-9.91963907309356E-17,4.5));
#6334=CARTESIAN_POINT('',(-0.81,-9.91963907309356E-17,4.5));
#6335=CARTESIAN_POINT('Origin',(0.,0.,4.5));
#6336=CARTESIAN_POINT('Origin',(0.,0.,4.5));
#6337=CARTESIAN_POINT('',(-1.1,-1.34711147906209E-16,5.5));
#6338=CARTESIAN_POINT('Origin',(0.,0.,5.5));
#6339=CARTESIAN_POINT('',(-1.1,-1.34711147906209E-16,4.5));
#6340=CARTESIAN_POINT('',(-1.1,-1.34711147906209E-16,4.5));
#6341=CARTESIAN_POINT('Origin',(0.,0.,4.5));
#6342=CARTESIAN_POINT('Origin',(0.,0.,5.5));
#6343=CARTESIAN_POINT('Origin',(0.,0.,4.5));
#6344=CARTESIAN_POINT('',(0.,0.,0.));
#6345=CARTESIAN_POINT('Origin',(0.,-2.5,12.));
#6346=CARTESIAN_POINT('',(-1.005,-1.7,12.));
#6347=CARTESIAN_POINT('Origin',(0.,-1.7,12.));
#6348=CARTESIAN_POINT('',(-1.005,-2.5,12.));
#6349=CARTESIAN_POINT('',(-1.005,-2.5,12.));
#6350=CARTESIAN_POINT('Origin',(0.,-2.5,12.));
#6351=CARTESIAN_POINT('Origin',(0.,-2.5,12.));
#6352=CARTESIAN_POINT('',(-1.4,-1.7,12.));
#6353=CARTESIAN_POINT('Origin',(0.,-1.7,12.));
#6354=CARTESIAN_POINT('',(-1.4,-2.5,12.));
#6355=CARTESIAN_POINT('',(-1.4,-2.5,12.));
#6356=CARTESIAN_POINT('Origin',(0.,-2.5,12.));
#6357=CARTESIAN_POINT('Origin',(0.,-1.7,12.));
#6358=CARTESIAN_POINT('Origin',(0.,-2.5,12.));
#6359=CARTESIAN_POINT('',(0.,0.,0.));
#6360=CARTESIAN_POINT('Origin',(0.173205080756888,-0.8,-0.3));
#6361=CARTESIAN_POINT('',(0.346410161513775,-0.8,0.));
#6362=CARTESIAN_POINT('',(0.173205080756888,-0.8,-0.3));
#6363=CARTESIAN_POINT('',(0.346410161513775,-0.8,0.));
#6364=CARTESIAN_POINT('',(0.173205080756888,-1.28,-0.3));
#6365=CARTESIAN_POINT('',(0.173205080756888,-0.8,-0.3));
#6366=CARTESIAN_POINT('',(0.346410161513775,-1.28,0.));
#6367=CARTESIAN_POINT('',(0.346410161513775,-1.28,0.));
#6368=CARTESIAN_POINT('',(0.346410161513775,-0.8,0.));
#6369=CARTESIAN_POINT('Origin',(-0.173205080756888,-0.8,-0.3));
#6370=CARTESIAN_POINT('',(-0.173205080756888,-0.8,-0.3));
#6371=CARTESIAN_POINT('',(0.173205080756888,-0.8,-0.3));
#6372=CARTESIAN_POINT('',(-0.173205080756888,-1.28,-0.3));
#6373=CARTESIAN_POINT('',(-0.173205080756888,-0.8,-0.3));
#6374=CARTESIAN_POINT('',(0.173205080756888,-1.28,-0.3));
#6375=CARTESIAN_POINT('Origin',(-0.346410161513775,-0.8,-5.55111512312578E-17));
#6376=CARTESIAN_POINT('',(-0.346410161513775,-0.8,-4.24230095489963E-17));
#6377=CARTESIAN_POINT('',(-0.173205080756888,-0.8,-0.3));
#6378=CARTESIAN_POINT('',(-0.346410161513775,-1.28,-5.55111512312578E-17));
#6379=CARTESIAN_POINT('',(-0.346410161513775,-0.8,-4.24230095489963E-17));
#6380=CARTESIAN_POINT('',(-0.173205080756888,-1.28,-0.3));
#6381=CARTESIAN_POINT('Origin',(-0.173205080756888,-0.8,0.3));
#6382=CARTESIAN_POINT('',(-0.173205080756888,-0.8,0.3));
#6383=CARTESIAN_POINT('',(-0.346410161513775,-0.8,-4.24230095489963E-17));
#6384=CARTESIAN_POINT('',(-0.173205080756888,-1.28,0.3));
#6385=CARTESIAN_POINT('',(-0.173205080756888,-0.8,0.3));
#6386=CARTESIAN_POINT('',(-0.346410161513775,-1.28,-4.24230095489963E-17));
#6387=CARTESIAN_POINT('Origin',(0.173205080756888,-0.8,0.3));
#6388=CARTESIAN_POINT('',(0.173205080756888,-0.8,0.3));
#6389=CARTESIAN_POINT('',(-0.173205080756888,-0.8,0.3));
#6390=CARTESIAN_POINT('',(0.173205080756888,-1.28,0.3));
#6391=CARTESIAN_POINT('',(0.173205080756888,-0.8,0.3));
#6392=CARTESIAN_POINT('',(-0.173205080756888,-1.28,0.3));
#6393=CARTESIAN_POINT('Origin',(0.346410161513775,-0.8,0.));
#6394=CARTESIAN_POINT('',(0.173205080756888,-0.8,0.3));
#6395=CARTESIAN_POINT('',(0.173205080756888,-1.28,0.3));
#6396=CARTESIAN_POINT('Origin',(0.,-0.8,-5.55111512312578E-17));
#6397=CARTESIAN_POINT('Origin',(0.,-1.28,-5.55111512312578E-17));
#6398=CARTESIAN_POINT('Origin',(0.,-2.9,0.));
#6399=CARTESIAN_POINT('',(-0.4,-2.9,4.89858719658941E-17));
#6400=CARTESIAN_POINT('Origin',(0.,-2.9,0.));
#6401=CARTESIAN_POINT('',(-0.3933,-2.9,4.81653586104654E-17));
#6402=CARTESIAN_POINT('Origin',(0.,-2.9,0.));
#6403=CARTESIAN_POINT('Origin',(0.,-7.5,0.));
#6404=CARTESIAN_POINT('',(-0.4,-7.5,4.89858719658941E-17));
#6405=CARTESIAN_POINT('',(-0.4,-7.5,4.89858719658941E-17));
#6406=CARTESIAN_POINT('Origin',(0.,-7.5,0.));
#6407=CARTESIAN_POINT('Origin',(0.,-7.5,0.));
#6408=CARTESIAN_POINT('Origin',(0.6,0.8,0.));
#6409=CARTESIAN_POINT('',(-0.6,0.8,-7.34788079488412E-17));
#6410=CARTESIAN_POINT('Origin',(0.,0.8,0.));
#6411=CARTESIAN_POINT('Origin',(0.,0.775,0.));
#6412=CARTESIAN_POINT('',(-0.65,0.75,-7.9602041944578E-17));
#6413=CARTESIAN_POINT('Origin',(0.,0.75,0.));
#6414=CARTESIAN_POINT('',(-0.625,0.775,-7.65404249467096E-17));
#6415=CARTESIAN_POINT('Origin',(0.,0.39,0.));
#6416=CARTESIAN_POINT('',(-0.65,0.0299999999999998,-7.9602041944578E-17));
#6417=CARTESIAN_POINT('Origin',(0.,0.0299999999999998,0.));
#6418=CARTESIAN_POINT('',(-0.65,0.39,-7.9602041944578E-17));
#6419=CARTESIAN_POINT('Origin',(0.,0.0150000000000001,0.));
#6420=CARTESIAN_POINT('',(-0.62,5.89805981832114E-17,-7.59281015471359E-17));
#6421=CARTESIAN_POINT('Origin',(0.,0.,0.));
#6422=CARTESIAN_POINT('',(-0.635,0.0150000000000001,-7.77650717458569E-17));
#6423=CARTESIAN_POINT('Origin',(0.42,0.,0.));
#6424=CARTESIAN_POINT('',(-0.42,-3.46944695195361E-18,-5.14351655641888E-17));
#6425=CARTESIAN_POINT('Origin',(0.,0.,0.));
#6426=CARTESIAN_POINT('Origin',(0.,-0.02,0.));
#6427=CARTESIAN_POINT('',(-0.3933,-0.0534000000000001,4.81653586104654E-17));
#6428=CARTESIAN_POINT('Origin',(0.,-0.0534000000000001,0.));
#6429=CARTESIAN_POINT('',(-0.41,-0.02,-5.02105187650415E-17));
#6430=CARTESIAN_POINT('Origin',(0.,-1.48,0.));
#6431=CARTESIAN_POINT('',(-0.3933,-1.48,-4.81653586104654E-17));
#6432=CARTESIAN_POINT('',(0.,0.,0.));
#6433=CARTESIAN_POINT('Origin',(0.,0.,0.));
#6434=CARTESIAN_POINT('',(-0.42,0.16,5.14351655641888E-17));
#6435=CARTESIAN_POINT('Origin',(0.,0.16,0.));
#6436=CARTESIAN_POINT('',(-0.42,0.,5.14351655641888E-17));
#6437=CARTESIAN_POINT('',(-0.42,0.,5.14351655641888E-17));
#6438=CARTESIAN_POINT('Origin',(0.,0.,0.));
#6439=CARTESIAN_POINT('Origin',(0.,0.,0.));
#6440=CARTESIAN_POINT('',(-0.8,0.16,9.79717439317883E-17));
#6441=CARTESIAN_POINT('Origin',(0.,0.16,0.));
#6442=CARTESIAN_POINT('',(-0.8,0.,9.79717439317883E-17));
#6443=CARTESIAN_POINT('',(-0.8,0.,9.79717439317883E-17));
#6444=CARTESIAN_POINT('Origin',(0.,0.,0.));
#6445=CARTESIAN_POINT('Origin',(0.,0.16,0.));
#6446=CARTESIAN_POINT('Origin',(0.,0.,0.));
#6447=CARTESIAN_POINT('',(0.,0.,0.));
#6448=CARTESIAN_POINT('Origin',(0.,0.067277284513851,0.));
#6449=CARTESIAN_POINT('',(-0.375277674973257,0.0768195421087395,0.65));
#6450=CARTESIAN_POINT('',(0.375277674973257,0.0768195421087395,0.65));
#6451=CARTESIAN_POINT('Ctrl Pts',(-0.375277674973257,0.0768195421087395,
0.65));
#6452=CARTESIAN_POINT('Ctrl Pts',(1.66533453693773E-13,-0.0315137912242439,
0.65));
#6453=CARTESIAN_POINT('Ctrl Pts',(0.375277674973257,0.0768195421087394,
0.65));
#6454=CARTESIAN_POINT('',(-0.750555349946514,0.0768195421087394,-9.19165206894919E-17));
#6455=CARTESIAN_POINT('Ctrl Pts',(-0.750555349946514,0.0768195421087394,
-9.19165206894919E-17));
#6456=CARTESIAN_POINT('Ctrl Pts',(-0.562916512459802,-0.0315137912242434,
0.325000000000144));
#6457=CARTESIAN_POINT('Ctrl Pts',(-0.375277674973257,0.0768195421087395,
0.65));
#6458=CARTESIAN_POINT('',(-0.6175,-2.77555756156289E-17,-7.5621939847349E-17));
#6459=CARTESIAN_POINT('',(-0.734027674973257,0.067277284513851,-8.98924642641573E-17));
#6460=CARTESIAN_POINT('Origin',(0.,0.,0.));
#6461=CARTESIAN_POINT('',(-0.375277674973257,0.0768195421087395,-0.65));
#6462=CARTESIAN_POINT('Ctrl Pts',(-0.375277674973257,0.0768195421087395,
-0.65));
#6463=CARTESIAN_POINT('Ctrl Pts',(-0.562916512459968,-0.0315137912242437,
-0.324999999999856));
#6464=CARTESIAN_POINT('Ctrl Pts',(-0.750555349946514,0.0768195421087395,
-9.19165206894919E-17));
#6465=CARTESIAN_POINT('',(0.375277674973257,0.0768195421087395,-0.65));
#6466=CARTESIAN_POINT('Ctrl Pts',(0.375277674973257,0.0768195421087395,
-0.65));
#6467=CARTESIAN_POINT('Ctrl Pts',(-1.66144875635155E-13,-0.0315137912242437,
-0.65));
#6468=CARTESIAN_POINT('Ctrl Pts',(-0.375277674973257,0.0768195421087395,
-0.65));
#6469=CARTESIAN_POINT('',(0.750555349946514,0.0768195421087394,0.));
#6470=CARTESIAN_POINT('Ctrl Pts',(0.750555349946514,0.0768195421087394,
0.));
#6471=CARTESIAN_POINT('Ctrl Pts',(0.562916512459802,-0.0315137912242436,
-0.325000000000144));
#6472=CARTESIAN_POINT('Ctrl Pts',(0.375277674973257,0.0768195421087395,
-0.65));
#6473=CARTESIAN_POINT('Ctrl Pts',(0.375277674973257,0.0768195421087394,
0.65));
#6474=CARTESIAN_POINT('Ctrl Pts',(0.562916512459968,-0.0315137912242439,
0.324999999999856));
#6475=CARTESIAN_POINT('Ctrl Pts',(0.750555349946514,0.0768195421087394,
0.));
#6476=CARTESIAN_POINT('Origin',(0.,0.612722715486149,0.));
#6477=CARTESIAN_POINT('',(-0.6175,0.68,-7.5621939847349E-17));
#6478=CARTESIAN_POINT('Origin',(0.,0.68,0.));
#6479=CARTESIAN_POINT('',(-0.750555349946514,0.603180457891261,-9.19165206894919E-17));
#6480=CARTESIAN_POINT('',(-0.734027674973257,0.612722715486149,-8.98924642641573E-17));
#6481=CARTESIAN_POINT('',(-0.375277674973257,0.603180457891261,0.65));
#6482=CARTESIAN_POINT('Ctrl Pts',(-0.375277674973257,0.603180457891261,
0.65));
#6483=CARTESIAN_POINT('Ctrl Pts',(-0.562916512459968,0.711513791224243,
0.324999999999856));
#6484=CARTESIAN_POINT('Ctrl Pts',(-0.750555349946514,0.603180457891261,
-9.19165206894919E-17));
#6485=CARTESIAN_POINT('',(0.375277674973257,0.603180457891261,0.65));
#6486=CARTESIAN_POINT('Ctrl Pts',(0.375277674973257,0.603180457891261,0.65));
#6487=CARTESIAN_POINT('Ctrl Pts',(-1.66755498298699E-13,0.711513791224244,
0.65));
#6488=CARTESIAN_POINT('Ctrl Pts',(-0.375277674973257,0.603180457891261,
0.65));
#6489=CARTESIAN_POINT('',(0.750555349946514,0.603180457891261,0.));
#6490=CARTESIAN_POINT('Ctrl Pts',(0.750555349946514,0.603180457891261,0.));
#6491=CARTESIAN_POINT('Ctrl Pts',(0.562916512459802,0.711513791224244,0.325000000000144));
#6492=CARTESIAN_POINT('Ctrl Pts',(0.375277674973257,0.603180457891261,0.65));
#6493=CARTESIAN_POINT('',(0.375277674973257,0.603180457891261,-0.65));
#6494=CARTESIAN_POINT('Ctrl Pts',(0.375277674973257,0.603180457891261,-0.65));
#6495=CARTESIAN_POINT('Ctrl Pts',(0.562916512459969,0.711513791224244,-0.324999999999856));
#6496=CARTESIAN_POINT('Ctrl Pts',(0.750555349946514,0.603180457891261,0.));
#6497=CARTESIAN_POINT('',(-0.375277674973257,0.603180457891261,-0.65));
#6498=CARTESIAN_POINT('Ctrl Pts',(-0.375277674973257,0.603180457891261,
-0.65));
#6499=CARTESIAN_POINT('Ctrl Pts',(1.66422431391311E-13,0.711513791224244,
-0.65));
#6500=CARTESIAN_POINT('Ctrl Pts',(0.375277674973257,0.603180457891261,-0.65));
#6501=CARTESIAN_POINT('Ctrl Pts',(-0.750555349946514,0.603180457891261,
-9.19165206894919E-17));
#6502=CARTESIAN_POINT('Ctrl Pts',(-0.562916512459802,0.711513791224244,
-0.325000000000144));
#6503=CARTESIAN_POINT('Ctrl Pts',(-0.375277674973257,0.603180457891261,
-0.65));
#6504=CARTESIAN_POINT('Origin',(0.375277674973257,0.,-0.65));
#6505=CARTESIAN_POINT('',(-0.375277674973257,0.,-0.65));
#6506=CARTESIAN_POINT('',(0.375277674973257,0.,-0.65));
#6507=CARTESIAN_POINT('Origin',(-0.375277674973257,0.,-0.65));
#6508=CARTESIAN_POINT('',(-0.750555349946514,0.,-9.19165206894919E-17));
#6509=CARTESIAN_POINT('Origin',(-0.750555349946514,0.,-9.19165206894919E-17));
#6510=CARTESIAN_POINT('',(-0.375277674973257,0.,0.65));
#6511=CARTESIAN_POINT('Origin',(0.,0.,0.));
#6512=CARTESIAN_POINT('',(-0.338975,0.68,4.15124648740974E-17));
#6513=CARTESIAN_POINT('Origin',(0.,0.68,0.));
#6514=CARTESIAN_POINT('',(-0.338975,0.,4.15124648740974E-17));
#6515=CARTESIAN_POINT('',(-0.338975,0.,4.15124648740974E-17));
#6516=CARTESIAN_POINT('Origin',(0.,0.,0.));
#6517=CARTESIAN_POINT('Origin',(-0.375277674973257,0.,0.65));
#6518=CARTESIAN_POINT('',(0.375277674973257,0.,0.65));
#6519=CARTESIAN_POINT('Origin',(0.750555349946514,0.,0.));
#6520=CARTESIAN_POINT('',(0.750555349946514,0.,0.));
#6521=CARTESIAN_POINT('Origin',(0.375277674973257,0.,0.65));
#6522=CARTESIAN_POINT('Origin',(0.,0.68,-1.11022302462516E-16));
#6523=CARTESIAN_POINT('Origin',(0.,0.,-1.11022302462516E-16));
#6524=CARTESIAN_POINT('',(0.,0.,0.));
#6525=CARTESIAN_POINT('Origin',(0.6,0.8,0.));
#6526=CARTESIAN_POINT('',(-0.6,0.8,-7.34788079488412E-17));
#6527=CARTESIAN_POINT('Origin',(0.,0.8,0.));
#6528=CARTESIAN_POINT('Origin',(0.,0.775,0.));
#6529=CARTESIAN_POINT('',(-0.65,0.75,-7.9602041944578E-17));
#6530=CARTESIAN_POINT('Origin',(0.,0.75,0.));
#6531=CARTESIAN_POINT('',(-0.625,0.775,-7.65404249467096E-17));
#6532=CARTESIAN_POINT('Origin',(0.,0.39,0.));
#6533=CARTESIAN_POINT('',(-0.65,0.0299999999999998,-7.9602041944578E-17));
#6534=CARTESIAN_POINT('Origin',(0.,0.0299999999999998,0.));
#6535=CARTESIAN_POINT('',(-0.65,0.39,-7.9602041944578E-17));
#6536=CARTESIAN_POINT('Origin',(0.,0.0150000000000001,0.));
#6537=CARTESIAN_POINT('',(-0.62,5.89805981832114E-17,-7.59281015471359E-17));
#6538=CARTESIAN_POINT('Origin',(0.,0.,0.));
#6539=CARTESIAN_POINT('',(-0.635,0.0150000000000001,-7.77650717458569E-17));
#6540=CARTESIAN_POINT('Origin',(0.42,0.,0.));
#6541=CARTESIAN_POINT('',(-0.42,-3.46944695195361E-18,-5.14351655641888E-17));
#6542=CARTESIAN_POINT('Origin',(0.,0.,0.));
#6543=CARTESIAN_POINT('Origin',(0.,-0.02,0.));
#6544=CARTESIAN_POINT('',(-0.3933,-0.0534000000000001,4.81653586104654E-17));
#6545=CARTESIAN_POINT('Origin',(0.,-0.0534000000000001,0.));
#6546=CARTESIAN_POINT('',(-0.41,-0.02,-5.02105187650415E-17));
#6547=CARTESIAN_POINT('Origin',(0.,-1.48,0.));
#6548=CARTESIAN_POINT('',(-0.3933,-2.9267,4.81653586104654E-17));
#6549=CARTESIAN_POINT('Origin',(0.,-2.9267,0.));
#6550=CARTESIAN_POINT('',(-0.3933,-1.48,-4.81653586104654E-17));
#6551=CARTESIAN_POINT('Origin',(0.,-2.96,0.));
#6552=CARTESIAN_POINT('',(-0.32,-3.,-3.91886975727153E-17));
#6553=CARTESIAN_POINT('Origin',(0.,-3.,0.));
#6554=CARTESIAN_POINT('',(-0.36,-2.96,-4.40872847693047E-17));
#6555=CARTESIAN_POINT('Origin',(0.,-3.,0.));
#6556=CARTESIAN_POINT('Origin',(0.173205080756888,-0.8,-0.3));
#6557=CARTESIAN_POINT('',(0.346410161513775,-0.8,0.));
#6558=CARTESIAN_POINT('',(0.173205080756888,-0.8,-0.3));
#6559=CARTESIAN_POINT('',(0.346410161513775,-0.8,0.));
#6560=CARTESIAN_POINT('',(0.173205080756888,-1.28,-0.3));
#6561=CARTESIAN_POINT('',(0.173205080756888,-0.8,-0.3));
#6562=CARTESIAN_POINT('',(0.346410161513775,-1.28,0.));
#6563=CARTESIAN_POINT('',(0.346410161513775,-1.28,0.));
#6564=CARTESIAN_POINT('',(0.346410161513775,-0.8,0.));
#6565=CARTESIAN_POINT('Origin',(-0.173205080756888,-0.8,-0.3));
#6566=CARTESIAN_POINT('',(-0.173205080756888,-0.8,-0.3));
#6567=CARTESIAN_POINT('',(0.173205080756888,-0.8,-0.3));
#6568=CARTESIAN_POINT('',(-0.173205080756888,-1.28,-0.3));
#6569=CARTESIAN_POINT('',(-0.173205080756888,-0.8,-0.3));
#6570=CARTESIAN_POINT('',(0.173205080756888,-1.28,-0.3));
#6571=CARTESIAN_POINT('Origin',(-0.346410161513775,-0.8,-5.55111512312578E-17));
#6572=CARTESIAN_POINT('',(-0.346410161513775,-0.8,-4.24230095489963E-17));
#6573=CARTESIAN_POINT('',(-0.173205080756888,-0.8,-0.3));
#6574=CARTESIAN_POINT('',(-0.346410161513775,-1.28,-5.55111512312578E-17));
#6575=CARTESIAN_POINT('',(-0.346410161513775,-0.8,-4.24230095489963E-17));
#6576=CARTESIAN_POINT('',(-0.173205080756888,-1.28,-0.3));
#6577=CARTESIAN_POINT('Origin',(-0.173205080756888,-0.8,0.3));
#6578=CARTESIAN_POINT('',(-0.173205080756888,-0.8,0.3));
#6579=CARTESIAN_POINT('',(-0.346410161513775,-0.8,-4.24230095489963E-17));
#6580=CARTESIAN_POINT('',(-0.173205080756888,-1.28,0.3));
#6581=CARTESIAN_POINT('',(-0.173205080756888,-0.8,0.3));
#6582=CARTESIAN_POINT('',(-0.346410161513775,-1.28,-4.24230095489963E-17));
#6583=CARTESIAN_POINT('Origin',(0.173205080756888,-0.8,0.3));
#6584=CARTESIAN_POINT('',(0.173205080756888,-0.8,0.3));
#6585=CARTESIAN_POINT('',(-0.173205080756888,-0.8,0.3));
#6586=CARTESIAN_POINT('',(0.173205080756888,-1.28,0.3));
#6587=CARTESIAN_POINT('',(0.173205080756888,-0.8,0.3));
#6588=CARTESIAN_POINT('',(-0.173205080756888,-1.28,0.3));
#6589=CARTESIAN_POINT('Origin',(0.346410161513775,-0.8,0.));
#6590=CARTESIAN_POINT('',(0.173205080756888,-0.8,0.3));
#6591=CARTESIAN_POINT('',(0.173205080756888,-1.28,0.3));
#6592=CARTESIAN_POINT('Origin',(0.,-0.8,-5.55111512312578E-17));
#6593=CARTESIAN_POINT('Origin',(0.,-1.28,-5.55111512312578E-17));
#6594=CARTESIAN_POINT('',(0.,0.,0.));
#6595=CARTESIAN_POINT('',(0.,0.,0.));
#6596=CARTESIAN_POINT('',(0.,0.,0.));
#6597=CARTESIAN_POINT('',(0.,0.,0.));
#6598=CARTESIAN_POINT('',(0.,0.,0.));
#6599=CARTESIAN_POINT('',(0.,0.,0.));
#6600=CARTESIAN_POINT('',(0.,0.,0.));
#6601=CARTESIAN_POINT('',(0.,0.,0.));
#6602=CARTESIAN_POINT('',(0.,0.,0.));
#6603=CARTESIAN_POINT('',(0.,4.2,0.));
#6604=CARTESIAN_POINT('',(-2.,3.1,5.));
#6605=CARTESIAN_POINT('',(-2.,3.26,5.));
#6606=CARTESIAN_POINT('',(-2.,-3.26,5.));
#6607=CARTESIAN_POINT('',(-2.,-3.94,5.));
#6608=CARTESIAN_POINT('',(2.,3.1,5.));
#6609=CARTESIAN_POINT('',(2.,3.26,5.));
#6610=CARTESIAN_POINT('',(2.,-3.26,5.));
#6611=CARTESIAN_POINT('',(2.,-3.94,5.));
#6612=CARTESIAN_POINT('',(0.,3.1,20.5));
#6613=CARTESIAN_POINT('',(0.,3.26,20.5));
#6614=CARTESIAN_POINT('',(0.,-3.26,20.5));
#6615=CARTESIAN_POINT('',(0.,-3.94,20.5));
#6616=CARTESIAN_POINT('',(0.,3.4,12.));
#6617=CARTESIAN_POINT('',(0.,0.,0.));
#6618=CARTESIAN_POINT('',(0.,0.,0.));
#6619=CARTESIAN_POINT('Origin',(-1.90918830920368,-2.1,10.0908116907963));
#6620=CARTESIAN_POINT('',(-2.07418830920368,-2.,10.0908116907963));
#6621=CARTESIAN_POINT('Origin',(-1.90918830920368,-2.,10.0908116907963));
#6622=CARTESIAN_POINT('',(-2.07418830920368,2.,10.0908116907963));
#6623=CARTESIAN_POINT('',(-2.07418830920368,-2.1,10.0908116907963));
#6624=CARTESIAN_POINT('Origin',(-1.90918830920368,2.,10.0908116907963));
#6625=CARTESIAN_POINT('Origin',(-1.90918830920368,-2.1,13.9091883092037));
#6626=CARTESIAN_POINT('',(-2.07418830920368,-2.,13.9091883092037));
#6627=CARTESIAN_POINT('Origin',(-1.90918830920368,-2.,13.9091883092037));
#6628=CARTESIAN_POINT('',(-2.07418830920368,2.,13.9091883092037));
#6629=CARTESIAN_POINT('',(-2.07418830920368,-2.1,13.9091883092037));
#6630=CARTESIAN_POINT('Origin',(-1.90918830920368,2.,13.9091883092037));
#6631=CARTESIAN_POINT('Origin',(1.90918830920368,-2.1,13.9091883092037));
#6632=CARTESIAN_POINT('',(1.74418830920368,-2.,13.9091883092037));
#6633=CARTESIAN_POINT('Origin',(1.90918830920368,-2.,13.9091883092037));
#6634=CARTESIAN_POINT('',(1.74418830920368,2.,13.9091883092037));
#6635=CARTESIAN_POINT('',(1.74418830920368,-2.1,13.9091883092037));
#6636=CARTESIAN_POINT('Origin',(1.90918830920368,2.,13.9091883092037));
#6637=CARTESIAN_POINT('Origin',(1.90918830920368,-2.1,10.0908116907963));
#6638=CARTESIAN_POINT('',(1.74418830920368,-2.,10.0908116907963));
#6639=CARTESIAN_POINT('Origin',(1.90918830920368,-2.,10.0908116907963));
#6640=CARTESIAN_POINT('',(1.74418830920368,2.,10.0908116907963));
#6641=CARTESIAN_POINT('',(1.74418830920368,-2.1,10.0908116907963));
#6642=CARTESIAN_POINT('Origin',(1.90918830920368,2.,10.0908116907963));
#6643=CARTESIAN_POINT('Origin',(0.,-0.3,12.));
#6644=CARTESIAN_POINT('',(-4.4,4.44089209850063E-16,12.));
#6645=CARTESIAN_POINT('Origin',(0.,0.,12.));
#6646=CARTESIAN_POINT('',(-5.,-0.6,12.));
#6647=CARTESIAN_POINT('',(-4.7,-0.3,12.));
#6648=CARTESIAN_POINT('Origin',(0.,-0.6,12.));
#6649=CARTESIAN_POINT('Origin',(0.,0.3,12.));
#6650=CARTESIAN_POINT('',(-5.,0.6,12.));
#6651=CARTESIAN_POINT('Origin',(0.,0.6,12.));
#6652=CARTESIAN_POINT('',(-4.7,0.3,12.));
#6653=CARTESIAN_POINT('Origin',(0.,-1.2,12.));
#6654=CARTESIAN_POINT('',(-5.,1.2,12.));
#6655=CARTESIAN_POINT('Origin',(0.,1.2,12.));
#6656=CARTESIAN_POINT('',(-5.,-1.2,12.));
#6657=CARTESIAN_POINT('Origin',(0.,1.2,12.));
#6658=CARTESIAN_POINT('',(-3.,1.2,12.));
#6659=CARTESIAN_POINT('Origin',(0.,1.2,12.));
#6660=CARTESIAN_POINT('Origin',(0.,-1.2,12.));
#6661=CARTESIAN_POINT('',(-5.,-1.2,12.));
#6662=CARTESIAN_POINT('Origin',(0.,-1.2,12.));
#6663=CARTESIAN_POINT('',(-3.,-1.2,12.));
#6664=CARTESIAN_POINT('Origin',(0.,-1.2,12.));
#6665=CARTESIAN_POINT('Origin',(0.,-1.2,12.));
#6666=CARTESIAN_POINT('',(-5.,-1.2,12.));
#6667=CARTESIAN_POINT('Origin',(0.,-2.,12.));
#6668=CARTESIAN_POINT('',(-3.,-2.,12.));
#6669=CARTESIAN_POINT('',(-3.,-2.,12.));
#6670=CARTESIAN_POINT('Origin',(0.,-2.,12.));
#6671=CARTESIAN_POINT('Origin',(0.,-2.,12.));
#6672=CARTESIAN_POINT('',(-2.35,2.,12.));
#6673=CARTESIAN_POINT('Origin',(0.,2.,12.));
#6674=CARTESIAN_POINT('',(-2.35,-2.,12.));
#6675=CARTESIAN_POINT('',(-2.35,-2.,12.));
#6676=CARTESIAN_POINT('Origin',(0.,-2.,12.));
#6677=CARTESIAN_POINT('Origin',(0.,-2.,12.));
#6678=CARTESIAN_POINT('',(-3.,2.,12.));
#6679=CARTESIAN_POINT('Origin',(0.,2.,12.));
#6680=CARTESIAN_POINT('',(-3.,-2.,12.));
#6681=CARTESIAN_POINT('Origin',(0.,2.,12.));
#6682=CARTESIAN_POINT('Origin',(0.,-2.,12.));
#6683=CARTESIAN_POINT('',(0.,0.,0.));
#6684=CARTESIAN_POINT('Origin',(0.,-0.3,12.));
#6685=CARTESIAN_POINT('',(-1.9,0.3,12.));
#6686=CARTESIAN_POINT('Origin',(0.,0.3,12.));
#6687=CARTESIAN_POINT('',(-1.9,-0.3,12.));
#6688=CARTESIAN_POINT('',(-1.9,-0.3,12.));
#6689=CARTESIAN_POINT('Origin',(0.,-0.3,12.));
#6690=CARTESIAN_POINT('Origin',(0.,-0.3,12.));
#6691=CARTESIAN_POINT('',(-2.34,0.3,12.));
#6692=CARTESIAN_POINT('Origin',(0.,0.3,12.));
#6693=CARTESIAN_POINT('',(-2.34,-0.3,12.));
#6694=CARTESIAN_POINT('',(-2.34,-0.3,12.));
#6695=CARTESIAN_POINT('Origin',(0.,-0.3,12.));
#6696=CARTESIAN_POINT('Origin',(0.,0.3,12.));
#6697=CARTESIAN_POINT('Origin',(0.,-0.3,12.));
#6698=CARTESIAN_POINT('',(0.,0.,0.));
#6699=CARTESIAN_POINT('',(0.,0.,0.));
#6700=CARTESIAN_POINT('Origin',(0.,0.,0.));
#6701=CARTESIAN_POINT('',(-1.63531,-0.410863395882378,-2.00267715711366E-16));
#6702=CARTESIAN_POINT('',(-2.00267715711366E-16,-0.410863395882378,1.63531));
#6703=CARTESIAN_POINT('Origin',(0.,-0.410863395882378,0.));
#6704=CARTESIAN_POINT('Origin',(0.,-0.410863395882378,0.));
#6705=CARTESIAN_POINT('',(-2.00267715711366E-16,0.410863395882378,1.63531));
#6706=CARTESIAN_POINT('Origin',(-2.05128338857182E-16,0.,1.675));
#6707=CARTESIAN_POINT('',(-1.63531,0.410863395882378,2.00267715711366E-16));
#6708=CARTESIAN_POINT('Origin',(0.,0.410863395882378,0.));
#6709=CARTESIAN_POINT('Origin',(0.,0.410863395882378,0.));
#6710=CARTESIAN_POINT('Origin',(0.,0.,0.));
#6711=CARTESIAN_POINT('',(-1.63531,0.7,-2.00267715711366E-16));
#6712=CARTESIAN_POINT('',(-1.63531,0.,-2.00267715711366E-16));
#6713=CARTESIAN_POINT('Origin',(0.,0.7,0.));
#6714=CARTESIAN_POINT('Origin',(0.,0.,0.));
#6715=CARTESIAN_POINT('',(-1.,-0.6,-1.22464679914735E-16));
#6716=CARTESIAN_POINT('Origin',(0.,-0.6,0.));
#6717=CARTESIAN_POINT('',(-1.,0.6,-1.22464679914735E-16));
#6718=CARTESIAN_POINT('',(-1.,0.,-1.22464679914735E-16));
#6719=CARTESIAN_POINT('Origin',(0.,0.6,0.));
#6720=CARTESIAN_POINT('Origin',(0.,0.65,0.));
#6721=CARTESIAN_POINT('',(-1.1,0.7,-1.34711147906209E-16));
#6722=CARTESIAN_POINT('',(-1.05,0.65,-1.28587913910472E-16));
#6723=CARTESIAN_POINT('Origin',(0.,0.7,0.));
#6724=CARTESIAN_POINT('Origin',(1.63531,0.7,0.));
#6725=CARTESIAN_POINT('Origin',(0.,0.,0.));
#6726=CARTESIAN_POINT('',(-1.63531,-0.7,-2.00267715711366E-16));
#6727=CARTESIAN_POINT('Origin',(0.,-0.7,0.));
#6728=CARTESIAN_POINT('',(-1.63531,0.,-2.00267715711366E-16));
#6729=CARTESIAN_POINT('Origin',(1.1,-0.7,0.));
#6730=CARTESIAN_POINT('',(-1.1,-0.7,-1.34711147906209E-16));
#6731=CARTESIAN_POINT('Origin',(0.,-0.7,0.));
#6732=CARTESIAN_POINT('Origin',(0.,-0.65,0.));
#6733=CARTESIAN_POINT('',(-1.05,-0.65,-1.28587913910472E-16));
#6734=CARTESIAN_POINT('',(0.,0.,0.));
#6735=CARTESIAN_POINT('Origin',(0.,0.,0.));
#6736=CARTESIAN_POINT('',(-1.71469,0.410863395882378,-2.09988962002998E-16));
#6737=CARTESIAN_POINT('',(-2.09988962002998E-16,0.410863395882378,1.71469));
#6738=CARTESIAN_POINT('Origin',(0.,0.410863395882378,0.));
#6739=CARTESIAN_POINT('Origin',(0.,0.410863395882378,0.));
#6740=CARTESIAN_POINT('',(-2.09988962002998E-16,-0.410863395882378,1.71469));
#6741=CARTESIAN_POINT('Origin',(-2.05128338857182E-16,0.,1.675));
#6742=CARTESIAN_POINT('',(-1.71469,-0.410863395882378,2.09988962002998E-16));
#6743=CARTESIAN_POINT('Origin',(0.,-0.410863395882378,0.));
#6744=CARTESIAN_POINT('Origin',(0.,-0.410863395882378,0.));
#6745=CARTESIAN_POINT('Origin',(0.,0.,0.));
#6746=CARTESIAN_POINT('',(-1.71469,-0.7,-2.09988962002998E-16));
#6747=CARTESIAN_POINT('Origin',(0.,-0.7,0.));
#6748=CARTESIAN_POINT('',(-1.71469,0.,-2.09988962002998E-16));
#6749=CARTESIAN_POINT('Origin',(2.25,0.7,0.));
#6750=CARTESIAN_POINT('',(-2.25,0.7,-2.75545529808154E-16));
#6751=CARTESIAN_POINT('Origin',(0.,0.7,0.));
#6752=CARTESIAN_POINT('',(-1.71469,0.7,-2.09988962002998E-16));
#6753=CARTESIAN_POINT('Origin',(0.,0.7,0.));
#6754=CARTESIAN_POINT('Origin',(0.,0.65,0.));
#6755=CARTESIAN_POINT('',(-2.35,0.6,-2.87791997799628E-16));
#6756=CARTESIAN_POINT('Origin',(0.,0.6,0.));
#6757=CARTESIAN_POINT('',(-2.3,0.65,-2.81668763803891E-16));
#6758=CARTESIAN_POINT('Origin',(0.,0.,0.));
#6759=CARTESIAN_POINT('',(-2.35,-0.6,-2.87791997799628E-16));
#6760=CARTESIAN_POINT('Origin',(0.,-0.6,0.));
#6761=CARTESIAN_POINT('',(-2.35,0.,-2.87791997799628E-16));
#6762=CARTESIAN_POINT('Origin',(0.,-0.65,0.));
#6763=CARTESIAN_POINT('',(-2.25,-0.7,-2.75545529808154E-16));
#6764=CARTESIAN_POINT('Origin',(0.,-0.7,0.));
#6765=CARTESIAN_POINT('',(-2.3,-0.65,-2.81668763803891E-16));
#6766=CARTESIAN_POINT('Origin',(1.71469,-0.7,0.));
#6767=CARTESIAN_POINT('Origin',(0.,0.,0.));
#6768=CARTESIAN_POINT('',(-1.71469,0.,-2.09988962002998E-16));
#6769=CARTESIAN_POINT('',(0.,0.,0.));
#6770=CARTESIAN_POINT('Origin',(1.675,0.,0.));
#6771=CARTESIAN_POINT('',(1.675,-2.97627328869245E-33,0.3969));
#6772=CARTESIAN_POINT('',(1.675,-2.97627328869245E-33,-0.3969));
#6773=CARTESIAN_POINT('Origin',(1.675,0.,0.));
#6774=CARTESIAN_POINT('Origin',(1.18440385848747,0.,-1.18440385848747));
#6775=CARTESIAN_POINT('',(1.46505453994041,3.1867025333467E-33,-0.903753177034526));
#6776=CARTESIAN_POINT('',(0.903753177034527,-9.13924911073161E-33,-1.46505453994041));
#6777=CARTESIAN_POINT('Origin',(1.18440385848747,0.,-1.18440385848747));
#6778=CARTESIAN_POINT('Origin',(1.02564169428591E-16,0.,-1.675));
#6779=CARTESIAN_POINT('',(0.3969,-2.97627328869246E-33,-1.675));
#6780=CARTESIAN_POINT('',(-0.3969,-2.97627328869245E-33,-1.675));
#6781=CARTESIAN_POINT('Origin',(1.02564169428591E-16,0.,-1.675));
#6782=CARTESIAN_POINT('Origin',(-1.18440385848747,0.,-1.18440385848747));
#6783=CARTESIAN_POINT('',(-0.903753177034526,3.1867025333467E-33,-1.46505453994041));
#6784=CARTESIAN_POINT('',(-1.46505453994041,-9.13924911073161E-33,-0.903753177034527));
#6785=CARTESIAN_POINT('Origin',(-1.18440385848747,0.,-1.18440385848747));
#6786=CARTESIAN_POINT('Origin',(-1.675,0.,-2.05128338857182E-16));
#6787=CARTESIAN_POINT('',(-1.675,-2.97627328869246E-33,-0.3969));
#6788=CARTESIAN_POINT('',(-1.675,-2.97627328869245E-33,0.3969));
#6789=CARTESIAN_POINT('Origin',(-1.675,0.,-2.05128338857182E-16));
#6790=CARTESIAN_POINT('Origin',(-1.18440385848747,0.,1.18440385848747));
#6791=CARTESIAN_POINT('',(-1.46505453994041,6.26819044436628E-33,0.903753177034526));
#6792=CARTESIAN_POINT('',(-0.903753177034527,-1.22207370217512E-32,1.46505453994041));
#6793=CARTESIAN_POINT('Origin',(-1.18440385848747,0.,1.18440385848747));
#6794=CARTESIAN_POINT('Origin',(-3.07692508285772E-16,0.,1.675));
#6795=CARTESIAN_POINT('',(-0.3969,-2.97627328869246E-33,1.675));
#6796=CARTESIAN_POINT('',(0.396899999999999,-2.97627328869245E-33,1.675));
#6797=CARTESIAN_POINT('Origin',(-3.07692508285772E-16,0.,1.675));
#6798=CARTESIAN_POINT('Origin',(1.18440385848747,0.,1.18440385848747));
#6799=CARTESIAN_POINT('',(0.903753177034526,9.34967835538585E-33,1.46505453994041));
#6800=CARTESIAN_POINT('',(1.46505453994041,-1.53022249327708E-32,0.903753177034527));
#6801=CARTESIAN_POINT('Origin',(1.18440385848747,0.,1.18440385848747));
#6802=CARTESIAN_POINT('',(0.,0.,0.));
#6803=CARTESIAN_POINT('Origin',(1.18440385848747,0.,1.18440385848747));
#6804=CARTESIAN_POINT('',(0.846804978391753,-0.07938,1.40825612658882));
#6805=CARTESIAN_POINT('',(1.40825612658882,-0.07938,0.846804978391754));
#6806=CARTESIAN_POINT('Ctrl Pts',(0.846804978391752,-0.0793800000000001,
1.40825612658882));
#6807=CARTESIAN_POINT('Ctrl Pts',(0.854205272175554,-0.123401821157026,
1.40380622184538));
#6808=CARTESIAN_POINT('Ctrl Pts',(0.867957148219441,-0.166543350814306,
1.39550172959303));
#6809=CARTESIAN_POINT('Ctrl Pts',(0.902193646979982,-0.237231147975234,
1.3735491215176));
#6810=CARTESIAN_POINT('Ctrl Pts',(0.920778333482564,-0.266264900654909,
1.36127834356734));
#6811=CARTESIAN_POINT('Ctrl Pts',(0.962485392528369,-0.317195968905306,
1.33211611256184));
#6812=CARTESIAN_POINT('Ctrl Pts',(0.985600426557816,-0.33909093068465,1.31521005565926));
#6813=CARTESIAN_POINT('Ctrl Pts',(1.03253285680459,-0.373586846396559,1.27866649102984));
#6814=CARTESIAN_POINT('Ctrl Pts',(1.05871835910697,-0.388086240756494,1.25722555095714));
#6815=CARTESIAN_POINT('Ctrl Pts',(1.11153475808518,-0.407068917407805,1.2107812086231));
#6816=CARTESIAN_POINT('Ctrl Pts',(1.13814686046673,-0.411552957311693,1.18575674747573));
#6817=CARTESIAN_POINT('Ctrl Pts',(1.18575674747573,-0.411552957311693,1.13814686046673));
#6818=CARTESIAN_POINT('Ctrl Pts',(1.2107812086231,-0.407068917407805,1.11153475808518));
#6819=CARTESIAN_POINT('Ctrl Pts',(1.25722555095713,-0.388086240756494,1.05871835910697));
#6820=CARTESIAN_POINT('Ctrl Pts',(1.27866649102984,-0.373586846396559,1.03253285680459));
#6821=CARTESIAN_POINT('Ctrl Pts',(1.31521005565926,-0.33909093068465,0.985600426557816));
#6822=CARTESIAN_POINT('Ctrl Pts',(1.33211611256184,-0.317195968905306,0.962485392528369));
#6823=CARTESIAN_POINT('Ctrl Pts',(1.36127834356734,-0.266264900654909,0.920778333482565));
#6824=CARTESIAN_POINT('Ctrl Pts',(1.3735491215176,-0.237231147975234,0.902193646979983));
#6825=CARTESIAN_POINT('Ctrl Pts',(1.39550172959303,-0.166543350814306,0.867957148219442));
#6826=CARTESIAN_POINT('Ctrl Pts',(1.40380622184538,-0.123401821157026,0.854205272175555));
#6827=CARTESIAN_POINT('Ctrl Pts',(1.40825612658882,-0.0793800000000001,
0.846804978391753));
#6828=CARTESIAN_POINT('',(0.886256117232623,-0.07938,1.45861320581289));
#6829=CARTESIAN_POINT('Origin',(1.18440385848747,-0.07938,1.18440385848747));
#6830=CARTESIAN_POINT('',(1.45861320581289,-0.07938,0.886256117232624));
#6831=CARTESIAN_POINT('Ctrl Pts',(1.45861320581289,-0.0793800000000001,
0.886256117232623));
#6832=CARTESIAN_POINT('Ctrl Pts',(1.45630208793976,-0.101649918886749,0.890059788636852));
#6833=CARTESIAN_POINT('Ctrl Pts',(1.45296717977858,-0.123823518623746,0.895520212222107));
#6834=CARTESIAN_POINT('Ctrl Pts',(1.43904931717599,-0.192480977588836,0.917859913453975));
#6835=CARTESIAN_POINT('Ctrl Pts',(1.4243271592157,-0.236152929235938,0.940896403863072));
#6836=CARTESIAN_POINT('Ctrl Pts',(1.39055359345152,-0.303141259068212,0.990027513266106));
#6837=CARTESIAN_POINT('Ctrl Pts',(1.36743459453896,-0.335108247315849,1.02199477007745));
#6838=CARTESIAN_POINT('Ctrl Pts',(1.32643091652006,-0.373243761060364,1.07446535104584));
#6839=CARTESIAN_POINT('Ctrl Pts',(1.30441816675528,-0.387888272594439,1.10126842659597));
#6840=CARTESIAN_POINT('Ctrl Pts',(1.25681160160691,-0.407041111792943,1.15530234155453));
#6841=CARTESIAN_POINT('Ctrl Pts',(1.23119764287622,-0.411552957311693,1.18251418313119));
#6842=CARTESIAN_POINT('Ctrl Pts',(1.18251418313119,-0.411552957311693,1.23119764287622));
#6843=CARTESIAN_POINT('Ctrl Pts',(1.15530234155453,-0.407041111792943,1.25681160160691));
#6844=CARTESIAN_POINT('Ctrl Pts',(1.10126842659597,-0.387888272594439,1.30441816675528));
#6845=CARTESIAN_POINT('Ctrl Pts',(1.07446535104584,-0.373243761060364,1.32643091652006));
#6846=CARTESIAN_POINT('Ctrl Pts',(1.02199477007745,-0.335108247315848,1.36743459453896));
#6847=CARTESIAN_POINT('Ctrl Pts',(0.990027513266105,-0.303141259068211,
1.39055359345152));
#6848=CARTESIAN_POINT('Ctrl Pts',(0.940896403863071,-0.236152929235937,
1.42432715921571));
#6849=CARTESIAN_POINT('Ctrl Pts',(0.917859913453974,-0.192480977588835,
1.43904931717599));
#6850=CARTESIAN_POINT('Ctrl Pts',(0.895520212222106,-0.123823518623745,
1.45296717977858));
#6851=CARTESIAN_POINT('Ctrl Pts',(0.890059788636851,-0.101649918886749,
1.45630208793976));
#6852=CARTESIAN_POINT('Ctrl Pts',(0.886256117232622,-0.0793800000000001,
1.45861320581289));
#6853=CARTESIAN_POINT('Origin',(1.18440385848747,-0.07938,1.18440385848747));
#6854=CARTESIAN_POINT('Origin',(0.,-0.27783,0.));
#6855=CARTESIAN_POINT('',(0.404717578595295,-0.07938,1.65807299932179));
#6856=CARTESIAN_POINT('Origin',(0.,-0.07938,0.));
#6857=CARTESIAN_POINT('',(-0.404717578595296,-0.07938,1.65807299932179));
#6858=CARTESIAN_POINT('Ctrl Pts',(0.404717578595296,-0.0793800000000001,
1.65807299932179));
#6859=CARTESIAN_POINT('Ctrl Pts',(0.400393769631747,-0.101649918886749,
1.65912839404491));
#6860=CARTESIAN_POINT('Ctrl Pts',(0.394174530911058,-0.123823518623745,
1.66063136041479));
#6861=CARTESIAN_POINT('Ctrl Pts',(0.368536561654407,-0.192480977588835,
1.66658649961961));
#6862=CARTESIAN_POINT('Ctrl Pts',(0.341837165343982,-0.236152929235937,
1.67246562047521));
#6863=CARTESIAN_POINT('Ctrl Pts',(0.283214707341173,-0.303141259068211,
1.68332504372461));
#6864=CARTESIAN_POINT('Ctrl Pts',(0.244262842368623,-0.335108247315849,
1.68958170688653));
#6865=CARTESIAN_POINT('Ctrl Pts',(0.178166559972324,-0.373243761060364,
1.69769003172132));
#6866=CARTESIAN_POINT('Ctrl Pts',(0.143648558862931,-0.387888272594439,
1.70107730356824));
#6867=CARTESIAN_POINT('Ctrl Pts',(0.0717778861362652,-0.407041111792943,
1.70562212620408));
#6868=CARTESIAN_POINT('Ctrl Pts',(0.0344244045173309,-0.411552957311693,
1.706752));
#6869=CARTESIAN_POINT('Ctrl Pts',(-0.0344244045173315,-0.411552957311693,
1.706752));
#6870=CARTESIAN_POINT('Ctrl Pts',(-0.0717778861362658,-0.407041111792943,
1.70562212620408));
#6871=CARTESIAN_POINT('Ctrl Pts',(-0.143648558862932,-0.387888272594439,
1.70107730356824));
#6872=CARTESIAN_POINT('Ctrl Pts',(-0.178166559972325,-0.373243761060364,
1.69769003172132));
#6873=CARTESIAN_POINT('Ctrl Pts',(-0.244262842368624,-0.335108247315849,
1.68958170688653));
#6874=CARTESIAN_POINT('Ctrl Pts',(-0.283214707341173,-0.303141259068212,
1.68332504372461));
#6875=CARTESIAN_POINT('Ctrl Pts',(-0.341837165343982,-0.236152929235937,
1.67246562047521));
#6876=CARTESIAN_POINT('Ctrl Pts',(-0.368536561654408,-0.192480977588835,
1.66658649961961));
#6877=CARTESIAN_POINT('Ctrl Pts',(-0.394174530911059,-0.123823518623745,
1.66063136041479));
#6878=CARTESIAN_POINT('Ctrl Pts',(-0.400393769631748,-0.101649918886749,
1.65912839404491));
#6879=CARTESIAN_POINT('Ctrl Pts',(-0.404717578595297,-0.0793800000000001,
1.65807299932179));
#6880=CARTESIAN_POINT('',(-0.886256117232624,-0.07938,1.45861320581289));
#6881=CARTESIAN_POINT('Origin',(0.,-0.07938,0.));
#6882=CARTESIAN_POINT('',(-1.45861320581289,-0.07938,0.886256117232623));
#6883=CARTESIAN_POINT('Ctrl Pts',(-0.886256117232623,-0.0793800000000001,
1.45861320581289));
#6884=CARTESIAN_POINT('Ctrl Pts',(-0.890059788636852,-0.101649918886749,
1.45630208793976));
#6885=CARTESIAN_POINT('Ctrl Pts',(-0.895520212222106,-0.123823518623745,
1.45296717977858));
#6886=CARTESIAN_POINT('Ctrl Pts',(-0.917859913453974,-0.192480977588835,
1.43904931717599));
#6887=CARTESIAN_POINT('Ctrl Pts',(-0.940896403863071,-0.236152929235937,
1.4243271592157));
#6888=CARTESIAN_POINT('Ctrl Pts',(-0.990027513266105,-0.303141259068211,
1.39055359345152));
#6889=CARTESIAN_POINT('Ctrl Pts',(-1.02199477007745,-0.335108247315848,
1.36743459453896));
#6890=CARTESIAN_POINT('Ctrl Pts',(-1.07446535104584,-0.373243761060364,
1.32643091652006));
#6891=CARTESIAN_POINT('Ctrl Pts',(-1.10126842659597,-0.387888272594439,
1.30441816675528));
#6892=CARTESIAN_POINT('Ctrl Pts',(-1.15530234155453,-0.407041111792943,
1.25681160160691));
#6893=CARTESIAN_POINT('Ctrl Pts',(-1.18251418313119,-0.411552957311693,
1.23119764287622));
#6894=CARTESIAN_POINT('Ctrl Pts',(-1.23119764287622,-0.411552957311693,
1.18251418313119));
#6895=CARTESIAN_POINT('Ctrl Pts',(-1.25681160160691,-0.407041111792943,
1.15530234155453));
#6896=CARTESIAN_POINT('Ctrl Pts',(-1.30441816675528,-0.387888272594439,
1.10126842659597));
#6897=CARTESIAN_POINT('Ctrl Pts',(-1.32643091652006,-0.373243761060365,
1.07446535104584));
#6898=CARTESIAN_POINT('Ctrl Pts',(-1.36743459453896,-0.335108247315849,
1.02199477007745));
#6899=CARTESIAN_POINT('Ctrl Pts',(-1.39055359345152,-0.303141259068212,
0.990027513266106));
#6900=CARTESIAN_POINT('Ctrl Pts',(-1.4243271592157,-0.236152929235938,0.940896403863071));
#6901=CARTESIAN_POINT('Ctrl Pts',(-1.43904931717599,-0.192480977588836,
0.917859913453974));
#6902=CARTESIAN_POINT('Ctrl Pts',(-1.45296717977858,-0.123823518623746,
0.895520212222106));
#6903=CARTESIAN_POINT('Ctrl Pts',(-1.45630208793976,-0.101649918886749,
0.890059788636852));
#6904=CARTESIAN_POINT('Ctrl Pts',(-1.45861320581289,-0.0793800000000001,
0.886256117232623));
#6905=CARTESIAN_POINT('',(-1.65807299932179,-0.07938,0.404717578595295));
#6906=CARTESIAN_POINT('Origin',(0.,-0.07938,0.));
#6907=CARTESIAN_POINT('',(-1.706752,-0.411552957311693,2.08591827245526E-16));
#6908=CARTESIAN_POINT('Ctrl Pts',(-1.65807299932179,-0.0793800000000001,
0.404717578595296));
#6909=CARTESIAN_POINT('Ctrl Pts',(-1.65912839404491,-0.101649918886749,
0.400393769631747));
#6910=CARTESIAN_POINT('Ctrl Pts',(-1.66063136041479,-0.123823518623745,
0.394174530911058));
#6911=CARTESIAN_POINT('Ctrl Pts',(-1.66658649961961,-0.192480977588835,
0.368536561654407));
#6912=CARTESIAN_POINT('Ctrl Pts',(-1.67246562047521,-0.236152929235937,
0.341837165343982));
#6913=CARTESIAN_POINT('Ctrl Pts',(-1.68332504372461,-0.303141259068211,
0.283214707341173));
#6914=CARTESIAN_POINT('Ctrl Pts',(-1.68958170688653,-0.335108247315848,
0.244262842368623));
#6915=CARTESIAN_POINT('Ctrl Pts',(-1.69769003172132,-0.373243761060364,
0.178166559972324));
#6916=CARTESIAN_POINT('Ctrl Pts',(-1.70107730356824,-0.387888272594439,
0.143648558862931));
#6917=CARTESIAN_POINT('Ctrl Pts',(-1.70562212620408,-0.407041111792943,
0.0717778861362656));
#6918=CARTESIAN_POINT('Ctrl Pts',(-1.706752,-0.411552957311693,0.0344244045173313));
#6919=CARTESIAN_POINT('Ctrl Pts',(-1.706752,-0.411552957311693,2.08166817117217E-16));
#6920=CARTESIAN_POINT('',(-1.706752,-0.47628,2.09016837373834E-16));
#6921=CARTESIAN_POINT('',(-1.706752,-0.27783,2.09016837373834E-16));
#6922=CARTESIAN_POINT('Origin',(0.,-0.47628,0.));
#6923=CARTESIAN_POINT('',(-1.65807299932179,-0.07938,-0.404717578595296));
#6924=CARTESIAN_POINT('Ctrl Pts',(-1.706752,-0.411552957311693,2.0122792321331E-16));
#6925=CARTESIAN_POINT('Ctrl Pts',(-1.706752,-0.411552957311693,-0.0344244045173309));
#6926=CARTESIAN_POINT('Ctrl Pts',(-1.70562212620408,-0.407041111792943,
-0.0717778861362652));
#6927=CARTESIAN_POINT('Ctrl Pts',(-1.70107730356824,-0.387888272594439,
-0.143648558862931));
#6928=CARTESIAN_POINT('Ctrl Pts',(-1.69769003172132,-0.373243761060365,
-0.178166559972324));
#6929=CARTESIAN_POINT('Ctrl Pts',(-1.68958170688653,-0.335108247315849,
-0.244262842368623));
#6930=CARTESIAN_POINT('Ctrl Pts',(-1.68332504372461,-0.303141259068212,
-0.283214707341173));
#6931=CARTESIAN_POINT('Ctrl Pts',(-1.67246562047521,-0.236152929235938,
-0.341837165343982));
#6932=CARTESIAN_POINT('Ctrl Pts',(-1.66658649961961,-0.192480977588836,
-0.368536561654407));
#6933=CARTESIAN_POINT('Ctrl Pts',(-1.66063136041479,-0.123823518623745,
-0.394174530911059));
#6934=CARTESIAN_POINT('Ctrl Pts',(-1.65912839404491,-0.101649918886749,
-0.400393769631748));
#6935=CARTESIAN_POINT('Ctrl Pts',(-1.65807299932179,-0.0793800000000001,
-0.404717578595296));
#6936=CARTESIAN_POINT('',(-1.45861320581289,-0.07938,-0.886256117232623));
#6937=CARTESIAN_POINT('Origin',(0.,-0.07938,0.));
#6938=CARTESIAN_POINT('',(-0.886256117232623,-0.07938,-1.45861320581289));
#6939=CARTESIAN_POINT('Ctrl Pts',(-1.45861320581289,-0.0793800000000001,
-0.886256117232623));
#6940=CARTESIAN_POINT('Ctrl Pts',(-1.45630208793976,-0.101649918886749,
-0.890059788636852));
#6941=CARTESIAN_POINT('Ctrl Pts',(-1.45296717977858,-0.123823518623745,
-0.895520212222106));
#6942=CARTESIAN_POINT('Ctrl Pts',(-1.43904931717599,-0.192480977588835,
-0.917859913453974));
#6943=CARTESIAN_POINT('Ctrl Pts',(-1.4243271592157,-0.236152929235937,-0.940896403863072));
#6944=CARTESIAN_POINT('Ctrl Pts',(-1.39055359345152,-0.303141259068212,
-0.990027513266106));
#6945=CARTESIAN_POINT('Ctrl Pts',(-1.36743459453896,-0.335108247315849,
-1.02199477007745));
#6946=CARTESIAN_POINT('Ctrl Pts',(-1.32643091652006,-0.373243761060364,
-1.07446535104584));
#6947=CARTESIAN_POINT('Ctrl Pts',(-1.30441816675528,-0.387888272594439,
-1.10126842659597));
#6948=CARTESIAN_POINT('Ctrl Pts',(-1.25681160160691,-0.407041111792943,
-1.15530234155453));
#6949=CARTESIAN_POINT('Ctrl Pts',(-1.23119764287622,-0.411552957311693,
-1.18251418313119));
#6950=CARTESIAN_POINT('Ctrl Pts',(-1.18251418313119,-0.411552957311693,
-1.23119764287622));
#6951=CARTESIAN_POINT('Ctrl Pts',(-1.15530234155453,-0.407041111792943,
-1.25681160160691));
#6952=CARTESIAN_POINT('Ctrl Pts',(-1.10126842659597,-0.387888272594439,
-1.30441816675528));
#6953=CARTESIAN_POINT('Ctrl Pts',(-1.07446535104584,-0.373243761060364,
-1.32643091652006));
#6954=CARTESIAN_POINT('Ctrl Pts',(-1.02199477007745,-0.335108247315848,
-1.36743459453896));
#6955=CARTESIAN_POINT('Ctrl Pts',(-0.990027513266105,-0.303141259068211,
-1.39055359345152));
#6956=CARTESIAN_POINT('Ctrl Pts',(-0.940896403863071,-0.236152929235936,
-1.42432715921571));
#6957=CARTESIAN_POINT('Ctrl Pts',(-0.917859913453974,-0.192480977588835,
-1.43904931717599));
#6958=CARTESIAN_POINT('Ctrl Pts',(-0.895520212222106,-0.123823518623745,
-1.45296717977858));
#6959=CARTESIAN_POINT('Ctrl Pts',(-0.890059788636851,-0.101649918886749,
-1.45630208793976));
#6960=CARTESIAN_POINT('Ctrl Pts',(-0.886256117232623,-0.0793800000000001,
-1.45861320581289));
#6961=CARTESIAN_POINT('',(-0.404717578595295,-0.07938,-1.65807299932179));
#6962=CARTESIAN_POINT('Origin',(0.,-0.07938,0.));
#6963=CARTESIAN_POINT('',(0.404717578595296,-0.07938,-1.65807299932179));
#6964=CARTESIAN_POINT('Ctrl Pts',(-0.404717578595296,-0.0793800000000001,
-1.65807299932179));
#6965=CARTESIAN_POINT('Ctrl Pts',(-0.400393769631747,-0.101649918886749,
-1.65912839404491));
#6966=CARTESIAN_POINT('Ctrl Pts',(-0.394174530911058,-0.123823518623746,
-1.66063136041479));
#6967=CARTESIAN_POINT('Ctrl Pts',(-0.368536561654407,-0.192480977588836,
-1.66658649961961));
#6968=CARTESIAN_POINT('Ctrl Pts',(-0.341837165343982,-0.236152929235938,
-1.67246562047521));
#6969=CARTESIAN_POINT('Ctrl Pts',(-0.283214707341173,-0.303141259068212,
-1.68332504372461));
#6970=CARTESIAN_POINT('Ctrl Pts',(-0.244262842368623,-0.335108247315849,
-1.68958170688653));
#6971=CARTESIAN_POINT('Ctrl Pts',(-0.178166559972324,-0.373243761060364,
-1.69769003172132));
#6972=CARTESIAN_POINT('Ctrl Pts',(-0.143648558862931,-0.387888272594439,
-1.70107730356824));
#6973=CARTESIAN_POINT('Ctrl Pts',(-0.0717778861362653,-0.407041111792943,
-1.70562212620408));
#6974=CARTESIAN_POINT('Ctrl Pts',(-0.034424404517331,-0.411552957311693,
-1.706752));
#6975=CARTESIAN_POINT('Ctrl Pts',(0.0344244045173312,-0.411552957311693,
-1.706752));
#6976=CARTESIAN_POINT('Ctrl Pts',(0.0717778861362655,-0.407041111792943,
-1.70562212620408));
#6977=CARTESIAN_POINT('Ctrl Pts',(0.143648558862931,-0.387888272594439,
-1.70107730356824));
#6978=CARTESIAN_POINT('Ctrl Pts',(0.178166559972324,-0.373243761060364,
-1.69769003172132));
#6979=CARTESIAN_POINT('Ctrl Pts',(0.244262842368623,-0.335108247315849,
-1.68958170688653));
#6980=CARTESIAN_POINT('Ctrl Pts',(0.283214707341173,-0.303141259068212,
-1.68332504372461));
#6981=CARTESIAN_POINT('Ctrl Pts',(0.341837165343982,-0.236152929235937,
-1.67246562047521));
#6982=CARTESIAN_POINT('Ctrl Pts',(0.368536561654407,-0.192480977588835,
-1.66658649961961));
#6983=CARTESIAN_POINT('Ctrl Pts',(0.394174530911059,-0.123823518623745,
-1.66063136041479));
#6984=CARTESIAN_POINT('Ctrl Pts',(0.400393769631748,-0.101649918886749,
-1.65912839404491));
#6985=CARTESIAN_POINT('Ctrl Pts',(0.404717578595296,-0.0793800000000001,
-1.65807299932179));
#6986=CARTESIAN_POINT('',(0.886256117232623,-0.07938,-1.45861320581289));
#6987=CARTESIAN_POINT('Origin',(0.,-0.07938,0.));
#6988=CARTESIAN_POINT('',(1.45861320581289,-0.07938,-0.886256117232623));
#6989=CARTESIAN_POINT('Ctrl Pts',(0.886256117232623,-0.0793800000000001,
-1.45861320581289));
#6990=CARTESIAN_POINT('Ctrl Pts',(0.890059788636852,-0.101649918886749,
-1.45630208793976));
#6991=CARTESIAN_POINT('Ctrl Pts',(0.895520212222106,-0.123823518623745,
-1.45296717977858));
#6992=CARTESIAN_POINT('Ctrl Pts',(0.917859913453974,-0.192480977588835,
-1.43904931717599));
#6993=CARTESIAN_POINT('Ctrl Pts',(0.940896403863072,-0.236152929235937,
-1.4243271592157));
#6994=CARTESIAN_POINT('Ctrl Pts',(0.990027513266106,-0.303141259068211,
-1.39055359345152));
#6995=CARTESIAN_POINT('Ctrl Pts',(1.02199477007745,-0.335108247315849,-1.36743459453896));
#6996=CARTESIAN_POINT('Ctrl Pts',(1.07446535104584,-0.373243761060364,-1.32643091652006));
#6997=CARTESIAN_POINT('Ctrl Pts',(1.10126842659597,-0.387888272594439,-1.30441816675528));
#6998=CARTESIAN_POINT('Ctrl Pts',(1.15530234155453,-0.407041111792943,-1.25681160160691));
#6999=CARTESIAN_POINT('Ctrl Pts',(1.18251418313119,-0.411552957311693,-1.23119764287622));
#7000=CARTESIAN_POINT('Ctrl Pts',(1.23119764287622,-0.411552957311693,-1.18251418313119));
#7001=CARTESIAN_POINT('Ctrl Pts',(1.25681160160691,-0.407041111792943,-1.15530234155453));
#7002=CARTESIAN_POINT('Ctrl Pts',(1.30441816675528,-0.387888272594439,-1.10126842659597));
#7003=CARTESIAN_POINT('Ctrl Pts',(1.32643091652006,-0.373243761060364,-1.07446535104584));
#7004=CARTESIAN_POINT('Ctrl Pts',(1.36743459453896,-0.335108247315849,-1.02199477007745));
#7005=CARTESIAN_POINT('Ctrl Pts',(1.39055359345152,-0.303141259068212,-0.990027513266105));
#7006=CARTESIAN_POINT('Ctrl Pts',(1.4243271592157,-0.236152929235937,-0.940896403863071));
#7007=CARTESIAN_POINT('Ctrl Pts',(1.43904931717599,-0.192480977588835,-0.917859913453974));
#7008=CARTESIAN_POINT('Ctrl Pts',(1.45296717977858,-0.123823518623745,-0.895520212222106));
#7009=CARTESIAN_POINT('Ctrl Pts',(1.45630208793976,-0.101649918886749,-0.890059788636852));
#7010=CARTESIAN_POINT('Ctrl Pts',(1.45861320581289,-0.0793800000000001,
-0.886256117232623));
#7011=CARTESIAN_POINT('',(1.65807299932179,-0.07938,-0.404717578595296));
#7012=CARTESIAN_POINT('Origin',(0.,-0.07938,0.));
#7013=CARTESIAN_POINT('',(1.65807299932179,-0.07938,0.404717578595296));
#7014=CARTESIAN_POINT('Ctrl Pts',(1.65807299932179,-0.0793800000000001,
-0.404717578595296));
#7015=CARTESIAN_POINT('Ctrl Pts',(1.65912839404491,-0.101649918886749,-0.400393769631747));
#7016=CARTESIAN_POINT('Ctrl Pts',(1.66063136041479,-0.123823518623745,-0.394174530911058));
#7017=CARTESIAN_POINT('Ctrl Pts',(1.66658649961961,-0.192480977588835,-0.368536561654407));
#7018=CARTESIAN_POINT('Ctrl Pts',(1.67246562047521,-0.236152929235937,-0.341837165343982));
#7019=CARTESIAN_POINT('Ctrl Pts',(1.68332504372461,-0.303141259068212,-0.283214707341173));
#7020=CARTESIAN_POINT('Ctrl Pts',(1.68958170688653,-0.335108247315849,-0.244262842368623));
#7021=CARTESIAN_POINT('Ctrl Pts',(1.69769003172132,-0.373243761060364,-0.178166559972324));
#7022=CARTESIAN_POINT('Ctrl Pts',(1.70107730356824,-0.387888272594439,-0.143648558862931));
#7023=CARTESIAN_POINT('Ctrl Pts',(1.70562212620408,-0.407041111792943,-0.0717778861362655));
#7024=CARTESIAN_POINT('Ctrl Pts',(1.706752,-0.411552957311693,-0.0344244045173312));
#7025=CARTESIAN_POINT('Ctrl Pts',(1.706752,-0.411552957311693,0.0344244045173312));
#7026=CARTESIAN_POINT('Ctrl Pts',(1.70562212620408,-0.407041111792943,0.0717778861362655));
#7027=CARTESIAN_POINT('Ctrl Pts',(1.70107730356824,-0.387888272594439,0.143648558862931));
#7028=CARTESIAN_POINT('Ctrl Pts',(1.69769003172132,-0.373243761060364,0.178166559972324));
#7029=CARTESIAN_POINT('Ctrl Pts',(1.68958170688653,-0.335108247315849,0.244262842368623));
#7030=CARTESIAN_POINT('Ctrl Pts',(1.68332504372461,-0.303141259068212,0.283214707341173));
#7031=CARTESIAN_POINT('Ctrl Pts',(1.67246562047521,-0.236152929235937,0.341837165343982));
#7032=CARTESIAN_POINT('Ctrl Pts',(1.66658649961961,-0.192480977588835,0.368536561654407));
#7033=CARTESIAN_POINT('Ctrl Pts',(1.66063136041479,-0.123823518623745,0.394174530911058));
#7034=CARTESIAN_POINT('Ctrl Pts',(1.65912839404491,-0.101649918886749,0.400393769631747));
#7035=CARTESIAN_POINT('Ctrl Pts',(1.65807299932179,-0.0793800000000001,
0.404717578595296));
#7036=CARTESIAN_POINT('Origin',(0.,-0.07938,0.));
#7037=CARTESIAN_POINT('Origin',(0.,-0.07938,0.));
#7038=CARTESIAN_POINT('',(0.397005914195118,-0.07938,1.59456899932179));
#7039=CARTESIAN_POINT('Origin',(0.,-0.07938,0.));
#7040=CARTESIAN_POINT('Origin',(-3.33066907387547E-16,-0.07938,1.675));
#7041=CARTESIAN_POINT('Origin',(-3.33066907387547E-16,0.,1.675));
#7042=CARTESIAN_POINT('',(-0.397005914195118,-0.07938,1.59456899932179));
#7043=CARTESIAN_POINT('Ctrl Pts',(-0.397005914195119,-0.0793800000000001,
1.59456899932179));
#7044=CARTESIAN_POINT('Ctrl Pts',(-0.3886265584581,-0.123401821157026,1.59665523941937));
#7045=CARTESIAN_POINT('Ctrl Pts',(-0.373030350867485,-0.166543350814306,
1.60050712143809));
#7046=CARTESIAN_POINT('Ctrl Pts',(-0.333298652394954,-0.237231147975234,
1.60919314384089));
#7047=CARTESIAN_POINT('Ctrl Pts',(-0.311480544243687,-0.266264900654909,
1.61365775139403));
#7048=CARTESIAN_POINT('Ctrl Pts',(-0.261368388670537,-0.317195968905306,
1.62252828437015));
#7049=CARTESIAN_POINT('Ctrl Pts',(-0.233069203882014,-0.33909093068465,
1.62691869420078));
#7050=CARTESIAN_POINT('Ctrl Pts',(-0.174042761838764,-0.373586846396559,
1.63426473152765));
#7051=CARTESIAN_POINT('Ctrl Pts',(-0.14036578147155,-0.388086240756494,
1.63761964365402));
#7052=CARTESIAN_POINT('Ctrl Pts',(-0.0701778381840615,-0.407068917407805,
1.64212536811722));
#7053=CARTESIAN_POINT('Ctrl Pts',(-0.0336652739555918,-0.411552957311693,
1.643248));
#7054=CARTESIAN_POINT('Ctrl Pts',(0.0336652739555913,-0.411552957311693,
1.643248));
#7055=CARTESIAN_POINT('Ctrl Pts',(0.070177838184061,-0.407068917407805,
1.64212536811722));
#7056=CARTESIAN_POINT('Ctrl Pts',(0.140365781471549,-0.388086240756494,
1.63761964365402));
#7057=CARTESIAN_POINT('Ctrl Pts',(0.174042761838763,-0.373586846396559,
1.63426473152765));
#7058=CARTESIAN_POINT('Ctrl Pts',(0.233069203882014,-0.33909093068465,1.62691869420078));
#7059=CARTESIAN_POINT('Ctrl Pts',(0.261368388670536,-0.317195968905306,
1.62252828437015));
#7060=CARTESIAN_POINT('Ctrl Pts',(0.311480544243686,-0.266264900654908,
1.61365775139403));
#7061=CARTESIAN_POINT('Ctrl Pts',(0.333298652394954,-0.237231147975234,
1.60919314384089));
#7062=CARTESIAN_POINT('Ctrl Pts',(0.373030350867484,-0.166543350814306,
1.60050712143809));
#7063=CARTESIAN_POINT('Ctrl Pts',(0.388626558458099,-0.123401821157026,
1.59665523941937));
#7064=CARTESIAN_POINT('Ctrl Pts',(0.397005914195118,-0.07938,1.59456899932179));
#7065=CARTESIAN_POINT('Origin',(-3.33066907387547E-16,-0.07938,1.675));
#7066=CARTESIAN_POINT('Origin',(0.,-0.07938,0.));
#7067=CARTESIAN_POINT('',(-0.846804978391754,-0.07938,1.40825612658882));
#7068=CARTESIAN_POINT('Origin',(0.,-0.07938,0.));
#7069=CARTESIAN_POINT('Origin',(-1.18440385848747,-0.07938,1.18440385848747));
#7070=CARTESIAN_POINT('Origin',(-1.18440385848747,0.,1.18440385848747));
#7071=CARTESIAN_POINT('',(-1.40825612658882,-0.07938,0.846804978391753));
#7072=CARTESIAN_POINT('Ctrl Pts',(-1.40825612658882,-0.0793800000000001,
0.846804978391753));
#7073=CARTESIAN_POINT('Ctrl Pts',(-1.40380622184538,-0.123401821157026,
0.854205272175555));
#7074=CARTESIAN_POINT('Ctrl Pts',(-1.39550172959303,-0.166543350814306,
0.867957148219442));
#7075=CARTESIAN_POINT('Ctrl Pts',(-1.3735491215176,-0.237231147975235,0.902193646979983));
#7076=CARTESIAN_POINT('Ctrl Pts',(-1.36127834356734,-0.266264900654909,
0.920778333482565));
#7077=CARTESIAN_POINT('Ctrl Pts',(-1.33211611256184,-0.317195968905306,
0.962485392528369));
#7078=CARTESIAN_POINT('Ctrl Pts',(-1.31521005565926,-0.339090930684651,
0.985600426557816));
#7079=CARTESIAN_POINT('Ctrl Pts',(-1.27866649102984,-0.373586846396559,
1.03253285680459));
#7080=CARTESIAN_POINT('Ctrl Pts',(-1.25722555095714,-0.388086240756494,
1.05871835910697));
#7081=CARTESIAN_POINT('Ctrl Pts',(-1.2107812086231,-0.407068917407805,1.11153475808518));
#7082=CARTESIAN_POINT('Ctrl Pts',(-1.18575674747573,-0.411552957311693,
1.13814686046673));
#7083=CARTESIAN_POINT('Ctrl Pts',(-1.13814686046673,-0.411552957311693,
1.18575674747573));
#7084=CARTESIAN_POINT('Ctrl Pts',(-1.11153475808518,-0.407068917407805,
1.2107812086231));
#7085=CARTESIAN_POINT('Ctrl Pts',(-1.05871835910697,-0.388086240756494,
1.25722555095714));
#7086=CARTESIAN_POINT('Ctrl Pts',(-1.03253285680459,-0.373586846396559,
1.27866649102984));
#7087=CARTESIAN_POINT('Ctrl Pts',(-0.985600426557816,-0.33909093068465,
1.31521005565926));
#7088=CARTESIAN_POINT('Ctrl Pts',(-0.962485392528369,-0.317195968905306,
1.33211611256184));
#7089=CARTESIAN_POINT('Ctrl Pts',(-0.920778333482565,-0.266264900654908,
1.36127834356734));
#7090=CARTESIAN_POINT('Ctrl Pts',(-0.902193646979983,-0.237231147975234,
1.3735491215176));
#7091=CARTESIAN_POINT('Ctrl Pts',(-0.867957148219442,-0.166543350814306,
1.39550172959303));
#7092=CARTESIAN_POINT('Ctrl Pts',(-0.854205272175555,-0.123401821157026,
1.40380622184538));
#7093=CARTESIAN_POINT('Ctrl Pts',(-0.846804978391753,-0.0793800000000001,
1.40825612658882));
#7094=CARTESIAN_POINT('Origin',(-1.18440385848747,-0.07938,1.18440385848747));
#7095=CARTESIAN_POINT('Origin',(0.,-0.07938,0.));
#7096=CARTESIAN_POINT('',(-1.59456899932179,-0.07938,0.397005914195118));
#7097=CARTESIAN_POINT('Origin',(0.,-0.07938,0.));
#7098=CARTESIAN_POINT('Origin',(-1.675,-0.07938,-2.22044604925031E-16));
#7099=CARTESIAN_POINT('Origin',(-1.675,0.,-2.22044604925031E-16));
#7100=CARTESIAN_POINT('',(-1.59456899932179,-0.07938,-0.397005914195118));
#7101=CARTESIAN_POINT('',(-1.643248,-0.411552957311693,3.47540551556327E-18));
#7102=CARTESIAN_POINT('Ctrl Pts',(-1.59456899932179,-0.0793800000000001,
-0.397005914195119));
#7103=CARTESIAN_POINT('Ctrl Pts',(-1.59665523941937,-0.123401821157026,
-0.388626558458099));
#7104=CARTESIAN_POINT('Ctrl Pts',(-1.60050712143809,-0.166543350814306,
-0.373030350867485));
#7105=CARTESIAN_POINT('Ctrl Pts',(-1.60919314384089,-0.237231147975234,
-0.333298652394954));
#7106=CARTESIAN_POINT('Ctrl Pts',(-1.61365775139403,-0.266264900654909,
-0.311480544243686));
#7107=CARTESIAN_POINT('Ctrl Pts',(-1.62252828437015,-0.317195968905306,
-0.261368388670537));
#7108=CARTESIAN_POINT('Ctrl Pts',(-1.62691869420078,-0.33909093068465,-0.233069203882014));
#7109=CARTESIAN_POINT('Ctrl Pts',(-1.63426473152765,-0.373586846396559,
-0.174042761838764));
#7110=CARTESIAN_POINT('Ctrl Pts',(-1.63761964365402,-0.388086240756494,
-0.140365781471549));
#7111=CARTESIAN_POINT('Ctrl Pts',(-1.64212536811722,-0.407068917407805,
-0.0701778381840614));
#7112=CARTESIAN_POINT('Ctrl Pts',(-1.643248,-0.411552957311693,-0.0336652739555917));
#7113=CARTESIAN_POINT('Ctrl Pts',(-1.643248,-0.411552957311693,-2.0122792321331E-16));
#7114=CARTESIAN_POINT('Origin',(-1.675,-0.07938,-2.22044604925031E-16));
#7115=CARTESIAN_POINT('Ctrl Pts',(-1.643248,-0.411552957311693,-1.94289029309402E-16));
#7116=CARTESIAN_POINT('Ctrl Pts',(-1.643248,-0.411552957311693,0.0336652739555913));
#7117=CARTESIAN_POINT('Ctrl Pts',(-1.64212536811722,-0.407068917407805,
0.0701778381840609));
#7118=CARTESIAN_POINT('Ctrl Pts',(-1.63761964365402,-0.388086240756494,
0.140365781471549));
#7119=CARTESIAN_POINT('Ctrl Pts',(-1.63426473152765,-0.373586846396559,
0.174042761838763));
#7120=CARTESIAN_POINT('Ctrl Pts',(-1.62691869420078,-0.33909093068465,0.233069203882014));
#7121=CARTESIAN_POINT('Ctrl Pts',(-1.62252828437015,-0.317195968905306,
0.261368388670536));
#7122=CARTESIAN_POINT('Ctrl Pts',(-1.61365775139403,-0.266264900654909,
0.311480544243686));
#7123=CARTESIAN_POINT('Ctrl Pts',(-1.60919314384089,-0.237231147975235,
0.333298652394954));
#7124=CARTESIAN_POINT('Ctrl Pts',(-1.60050712143809,-0.166543350814306,
0.373030350867484));
#7125=CARTESIAN_POINT('Ctrl Pts',(-1.59665523941937,-0.123401821157026,
0.388626558458099));
#7126=CARTESIAN_POINT('Ctrl Pts',(-1.59456899932179,-0.0793800000000001,
0.397005914195118));
#7127=CARTESIAN_POINT('Origin',(0.,-0.07938,0.));
#7128=CARTESIAN_POINT('',(-1.40825612658882,-0.07938,-0.846804978391753));
#7129=CARTESIAN_POINT('Origin',(0.,-0.07938,0.));
#7130=CARTESIAN_POINT('Origin',(-1.18440385848747,-0.07938,-1.18440385848747));
#7131=CARTESIAN_POINT('Origin',(-1.18440385848747,0.,-1.18440385848747));
#7132=CARTESIAN_POINT('',(-0.846804978391753,-0.07938,-1.40825612658882));
#7133=CARTESIAN_POINT('Ctrl Pts',(-0.846804978391753,-0.0793800000000001,
-1.40825612658882));
#7134=CARTESIAN_POINT('Ctrl Pts',(-0.854205272175555,-0.123401821157026,
-1.40380622184538));
#7135=CARTESIAN_POINT('Ctrl Pts',(-0.867957148219442,-0.166543350814306,
-1.39550172959303));
#7136=CARTESIAN_POINT('Ctrl Pts',(-0.902193646979982,-0.237231147975234,
-1.3735491215176));
#7137=CARTESIAN_POINT('Ctrl Pts',(-0.920778333482564,-0.266264900654908,
-1.36127834356734));
#7138=CARTESIAN_POINT('Ctrl Pts',(-0.962485392528368,-0.317195968905306,
-1.33211611256184));
#7139=CARTESIAN_POINT('Ctrl Pts',(-0.985600426557816,-0.33909093068465,
-1.31521005565926));
#7140=CARTESIAN_POINT('Ctrl Pts',(-1.03253285680459,-0.373586846396559,
-1.27866649102984));
#7141=CARTESIAN_POINT('Ctrl Pts',(-1.05871835910697,-0.388086240756494,
-1.25722555095714));
#7142=CARTESIAN_POINT('Ctrl Pts',(-1.11153475808518,-0.407068917407805,
-1.2107812086231));
#7143=CARTESIAN_POINT('Ctrl Pts',(-1.13814686046673,-0.411552957311693,
-1.18575674747573));
#7144=CARTESIAN_POINT('Ctrl Pts',(-1.18575674747573,-0.411552957311693,
-1.13814686046673));
#7145=CARTESIAN_POINT('Ctrl Pts',(-1.2107812086231,-0.407068917407805,-1.11153475808518));
#7146=CARTESIAN_POINT('Ctrl Pts',(-1.25722555095714,-0.388086240756494,
-1.05871835910697));
#7147=CARTESIAN_POINT('Ctrl Pts',(-1.27866649102984,-0.373586846396559,
-1.03253285680459));
#7148=CARTESIAN_POINT('Ctrl Pts',(-1.31521005565926,-0.33909093068465,-0.985600426557816));
#7149=CARTESIAN_POINT('Ctrl Pts',(-1.33211611256184,-0.317195968905306,
-0.962485392528369));
#7150=CARTESIAN_POINT('Ctrl Pts',(-1.36127834356734,-0.266264900654909,
-0.920778333482565));
#7151=CARTESIAN_POINT('Ctrl Pts',(-1.3735491215176,-0.237231147975234,-0.902193646979983));
#7152=CARTESIAN_POINT('Ctrl Pts',(-1.39550172959303,-0.166543350814306,
-0.867957148219442));
#7153=CARTESIAN_POINT('Ctrl Pts',(-1.40380622184538,-0.123401821157026,
-0.854205272175555));
#7154=CARTESIAN_POINT('Ctrl Pts',(-1.40825612658882,-0.07938,-0.846804978391753));
#7155=CARTESIAN_POINT('Origin',(-1.18440385848747,-0.07938,-1.18440385848747));
#7156=CARTESIAN_POINT('Origin',(0.,-0.07938,0.));
#7157=CARTESIAN_POINT('',(-0.397005914195118,-0.07938,-1.59456899932179));
#7158=CARTESIAN_POINT('Origin',(0.,-0.07938,0.));
#7159=CARTESIAN_POINT('Origin',(1.11022302462516E-16,-0.07938,-1.675));
#7160=CARTESIAN_POINT('Origin',(1.11022302462516E-16,0.,-1.675));
#7161=CARTESIAN_POINT('',(0.397005914195118,-0.07938,-1.59456899932179));
#7162=CARTESIAN_POINT('Ctrl Pts',(0.397005914195119,-0.0793800000000001,
-1.59456899932179));
#7163=CARTESIAN_POINT('Ctrl Pts',(0.388626558458099,-0.123401821157026,
-1.59665523941937));
#7164=CARTESIAN_POINT('Ctrl Pts',(0.373030350867485,-0.166543350814306,
-1.60050712143809));
#7165=CARTESIAN_POINT('Ctrl Pts',(0.333298652394954,-0.237231147975234,
-1.60919314384089));
#7166=CARTESIAN_POINT('Ctrl Pts',(0.311480544243686,-0.266264900654909,
-1.61365775139403));
#7167=CARTESIAN_POINT('Ctrl Pts',(0.261368388670537,-0.317195968905306,
-1.62252828437015));
#7168=CARTESIAN_POINT('Ctrl Pts',(0.233069203882014,-0.33909093068465,-1.62691869420078));
#7169=CARTESIAN_POINT('Ctrl Pts',(0.174042761838763,-0.373586846396559,
-1.63426473152765));
#7170=CARTESIAN_POINT('Ctrl Pts',(0.140365781471549,-0.388086240756494,
-1.63761964365402));
#7171=CARTESIAN_POINT('Ctrl Pts',(0.0701778381840612,-0.407068917407805,
-1.64212536811722));
#7172=CARTESIAN_POINT('Ctrl Pts',(0.0336652739555916,-0.411552957311693,
-1.643248));
#7173=CARTESIAN_POINT('Ctrl Pts',(-0.0336652739555915,-0.411552957311693,
-1.643248));
#7174=CARTESIAN_POINT('Ctrl Pts',(-0.0701778381840612,-0.407068917407805,
-1.64212536811722));
#7175=CARTESIAN_POINT('Ctrl Pts',(-0.140365781471549,-0.388086240756494,
-1.63761964365402));
#7176=CARTESIAN_POINT('Ctrl Pts',(-0.174042761838764,-0.373586846396559,
-1.63426473152765));
#7177=CARTESIAN_POINT('Ctrl Pts',(-0.233069203882014,-0.33909093068465,
-1.62691869420078));
#7178=CARTESIAN_POINT('Ctrl Pts',(-0.261368388670536,-0.317195968905306,
-1.62252828437015));
#7179=CARTESIAN_POINT('Ctrl Pts',(-0.311480544243686,-0.266264900654908,
-1.61365775139403));
#7180=CARTESIAN_POINT('Ctrl Pts',(-0.333298652394954,-0.237231147975234,
-1.60919314384089));
#7181=CARTESIAN_POINT('Ctrl Pts',(-0.373030350867485,-0.166543350814306,
-1.60050712143809));
#7182=CARTESIAN_POINT('Ctrl Pts',(-0.388626558458099,-0.123401821157026,
-1.59665523941937));
#7183=CARTESIAN_POINT('Ctrl Pts',(-0.397005914195118,-0.07938,-1.59456899932179));
#7184=CARTESIAN_POINT('Origin',(1.11022302462516E-16,-0.07938,-1.675));
#7185=CARTESIAN_POINT('Origin',(0.,-0.07938,0.));
#7186=CARTESIAN_POINT('',(0.846804978391753,-0.07938,-1.40825612658882));
#7187=CARTESIAN_POINT('Origin',(0.,-0.07938,0.));
#7188=CARTESIAN_POINT('Origin',(1.18440385848747,-0.07938,-1.18440385848747));
#7189=CARTESIAN_POINT('Origin',(1.18440385848747,0.,-1.18440385848747));
#7190=CARTESIAN_POINT('',(1.40825612658882,-0.07938,-0.846804978391753));
#7191=CARTESIAN_POINT('Ctrl Pts',(1.40825612658882,-0.0793800000000001,
-0.846804978391753));
#7192=CARTESIAN_POINT('Ctrl Pts',(1.40380622184538,-0.123401821157026,-0.854205272175555));
#7193=CARTESIAN_POINT('Ctrl Pts',(1.39550172959303,-0.166543350814306,-0.867957148219442));
#7194=CARTESIAN_POINT('Ctrl Pts',(1.3735491215176,-0.237231147975234,-0.902193646979983));
#7195=CARTESIAN_POINT('Ctrl Pts',(1.36127834356734,-0.266264900654908,-0.920778333482565));
#7196=CARTESIAN_POINT('Ctrl Pts',(1.33211611256184,-0.317195968905306,-0.962485392528369));
#7197=CARTESIAN_POINT('Ctrl Pts',(1.31521005565926,-0.33909093068465,-0.985600426557816));
#7198=CARTESIAN_POINT('Ctrl Pts',(1.27866649102984,-0.373586846396559,-1.03253285680459));
#7199=CARTESIAN_POINT('Ctrl Pts',(1.25722555095714,-0.388086240756494,-1.05871835910697));
#7200=CARTESIAN_POINT('Ctrl Pts',(1.2107812086231,-0.407068917407805,-1.11153475808518));
#7201=CARTESIAN_POINT('Ctrl Pts',(1.18575674747573,-0.411552957311693,-1.13814686046673));
#7202=CARTESIAN_POINT('Ctrl Pts',(1.13814686046673,-0.411552957311693,-1.18575674747573));
#7203=CARTESIAN_POINT('Ctrl Pts',(1.11153475808518,-0.407068917407805,-1.2107812086231));
#7204=CARTESIAN_POINT('Ctrl Pts',(1.05871835910697,-0.388086240756494,-1.25722555095714));
#7205=CARTESIAN_POINT('Ctrl Pts',(1.03253285680459,-0.373586846396559,-1.27866649102984));
#7206=CARTESIAN_POINT('Ctrl Pts',(0.985600426557816,-0.33909093068465,-1.31521005565926));
#7207=CARTESIAN_POINT('Ctrl Pts',(0.962485392528369,-0.317195968905306,
-1.33211611256184));
#7208=CARTESIAN_POINT('Ctrl Pts',(0.920778333482565,-0.266264900654909,
-1.36127834356734));
#7209=CARTESIAN_POINT('Ctrl Pts',(0.902193646979983,-0.237231147975234,
-1.3735491215176));
#7210=CARTESIAN_POINT('Ctrl Pts',(0.867957148219442,-0.166543350814306,
-1.39550172959303));
#7211=CARTESIAN_POINT('Ctrl Pts',(0.854205272175555,-0.123401821157026,
-1.40380622184538));
#7212=CARTESIAN_POINT('Ctrl Pts',(0.846804978391753,-0.0793800000000001,
-1.40825612658882));
#7213=CARTESIAN_POINT('Origin',(1.18440385848747,-0.07938,-1.18440385848747));
#7214=CARTESIAN_POINT('Origin',(0.,-0.27783,0.));
#7215=CARTESIAN_POINT('',(-1.643248,-0.47628,2.01239840340529E-16));
#7216=CARTESIAN_POINT('Origin',(0.,-0.47628,0.));
#7217=CARTESIAN_POINT('',(-1.643248,-0.27783,2.01239840340529E-16));
#7218=CARTESIAN_POINT('',(1.59456899932179,-0.07938,0.397005914195118));
#7219=CARTESIAN_POINT('Origin',(0.,-0.07938,0.));
#7220=CARTESIAN_POINT('',(1.59456899932179,-0.07938,-0.397005914195118));
#7221=CARTESIAN_POINT('Ctrl Pts',(1.59456899932179,-0.0793800000000001,
0.397005914195118));
#7222=CARTESIAN_POINT('Ctrl Pts',(1.59665523941937,-0.123401821157026,0.388626558458099));
#7223=CARTESIAN_POINT('Ctrl Pts',(1.60050712143809,-0.166543350814306,0.373030350867485));
#7224=CARTESIAN_POINT('Ctrl Pts',(1.60919314384089,-0.237231147975234,0.333298652394954));
#7225=CARTESIAN_POINT('Ctrl Pts',(1.61365775139403,-0.266264900654909,0.311480544243686));
#7226=CARTESIAN_POINT('Ctrl Pts',(1.62252828437015,-0.317195968905306,0.261368388670537));
#7227=CARTESIAN_POINT('Ctrl Pts',(1.62691869420078,-0.33909093068465,0.233069203882014));
#7228=CARTESIAN_POINT('Ctrl Pts',(1.63426473152765,-0.373586846396559,0.174042761838764));
#7229=CARTESIAN_POINT('Ctrl Pts',(1.63761964365402,-0.388086240756494,0.140365781471549));
#7230=CARTESIAN_POINT('Ctrl Pts',(1.64212536811722,-0.407068917407805,0.0701778381840612));
#7231=CARTESIAN_POINT('Ctrl Pts',(1.643248,-0.411552957311693,0.0336652739555916));
#7232=CARTESIAN_POINT('Ctrl Pts',(1.643248,-0.411552957311693,-0.0336652739555916));
#7233=CARTESIAN_POINT('Ctrl Pts',(1.64212536811722,-0.407068917407805,-0.0701778381840612));
#7234=CARTESIAN_POINT('Ctrl Pts',(1.63761964365402,-0.388086240756494,-0.140365781471549));
#7235=CARTESIAN_POINT('Ctrl Pts',(1.63426473152765,-0.373586846396559,-0.174042761838764));
#7236=CARTESIAN_POINT('Ctrl Pts',(1.62691869420078,-0.33909093068465,-0.233069203882014));
#7237=CARTESIAN_POINT('Ctrl Pts',(1.62252828437015,-0.317195968905306,-0.261368388670537));
#7238=CARTESIAN_POINT('Ctrl Pts',(1.61365775139403,-0.266264900654909,-0.311480544243686));
#7239=CARTESIAN_POINT('Ctrl Pts',(1.60919314384089,-0.237231147975234,-0.333298652394954));
#7240=CARTESIAN_POINT('Ctrl Pts',(1.60050712143809,-0.166543350814306,-0.373030350867485));
#7241=CARTESIAN_POINT('Ctrl Pts',(1.59665523941937,-0.123401821157026,-0.388626558458099));
#7242=CARTESIAN_POINT('Ctrl Pts',(1.59456899932179,-0.07938,-0.397005914195118));
#7243=CARTESIAN_POINT('Origin',(0.,-0.07938,0.));
#7244=CARTESIAN_POINT('Origin',(0.,-0.07938,0.));
#7245=CARTESIAN_POINT('Origin',(1.675,-0.07938,0.));
#7246=CARTESIAN_POINT('Origin',(1.675,0.,0.));
#7247=CARTESIAN_POINT('Origin',(1.675,-0.07938,0.));
#7248=CARTESIAN_POINT('Origin',(0.,-0.47628,0.));
#7249=CARTESIAN_POINT('Origin',(0.,-0.07938,0.));
#7250=CARTESIAN_POINT('',(0.,0.,0.));
#7251=CARTESIAN_POINT('Origin',(1.70469,0.695,0.));
#7252=CARTESIAN_POINT('',(-1.70469,0.695,-2.0876431520385E-16));
#7253=CARTESIAN_POINT('Origin',(0.,0.695,0.));
#7254=CARTESIAN_POINT('',(-1.65031,0.695,-2.02104685910087E-16));
#7255=CARTESIAN_POINT('Origin',(0.,0.695,0.));
#7256=CARTESIAN_POINT('Origin',(0.,0.6575,0.));
#7257=CARTESIAN_POINT('',(-1.70469,0.62,-2.0876431520385E-16));
#7258=CARTESIAN_POINT('Origin',(0.,0.62,0.));
#7259=CARTESIAN_POINT('',(-1.70469,0.6575,-2.0876431520385E-16));
#7260=CARTESIAN_POINT('Origin',(1.65031,0.62,0.));
#7261=CARTESIAN_POINT('',(-1.65031,0.62,-2.02104685910087E-16));
#7262=CARTESIAN_POINT('Origin',(0.,0.62,0.));
#7263=CARTESIAN_POINT('Origin',(0.,0.6575,0.));
#7264=CARTESIAN_POINT('',(-1.65031,0.6575,-2.02104685910087E-16));
#7265=CARTESIAN_POINT('Origin',(1.70469,-0.62,0.));
#7266=CARTESIAN_POINT('',(-1.70469,-0.62,-2.0876431520385E-16));
#7267=CARTESIAN_POINT('Origin',(0.,-0.62,0.));
#7268=CARTESIAN_POINT('',(-1.65031,-0.62,-2.02104685910087E-16));
#7269=CARTESIAN_POINT('Origin',(0.,-0.62,0.));
#7270=CARTESIAN_POINT('Origin',(0.,-0.6575,0.));
#7271=CARTESIAN_POINT('',(-1.70469,-0.695,-2.0876431520385E-16));
#7272=CARTESIAN_POINT('Origin',(0.,-0.695,0.));
#7273=CARTESIAN_POINT('',(-1.70469,-0.6575,-2.0876431520385E-16));
#7274=CARTESIAN_POINT('Origin',(1.65031,-0.695,0.));
#7275=CARTESIAN_POINT('',(-1.65031,-0.695,-2.02104685910087E-16));
#7276=CARTESIAN_POINT('Origin',(0.,-0.695,0.));
#7277=CARTESIAN_POINT('Origin',(0.,-0.6575,0.));
#7278=CARTESIAN_POINT('',(-1.65031,-0.6575,-2.02104685910087E-16));
#7279=CARTESIAN_POINT('',(0.,0.,0.));
#7280=CARTESIAN_POINT('',(0.,0.,0.));
#7281=CARTESIAN_POINT('',(0.,0.,0.));
#7282=CARTESIAN_POINT('',(0.,0.,0.));
#7283=CARTESIAN_POINT('',(0.,0.,0.));
#7284=CARTESIAN_POINT('',(0.,0.,0.));
#7285=CARTESIAN_POINT('Origin',(-1.90918830920368,-2.4,10.0908116907963));
#7286=CARTESIAN_POINT('',(-2.13418830920368,-2.3,10.0908116907963));
#7287=CARTESIAN_POINT('Origin',(-1.90918830920368,-2.3,10.0908116907963));
#7288=CARTESIAN_POINT('',(-2.13418830920368,-2.,10.0908116907963));
#7289=CARTESIAN_POINT('',(-2.13418830920368,-2.4,10.0908116907963));
#7290=CARTESIAN_POINT('Origin',(-1.90918830920368,-2.,10.0908116907963));
#7291=CARTESIAN_POINT('Origin',(-1.90918830920368,-2.4,13.9091883092037));
#7292=CARTESIAN_POINT('',(-2.13418830920368,-2.3,13.9091883092037));
#7293=CARTESIAN_POINT('Origin',(-1.90918830920368,-2.3,13.9091883092037));
#7294=CARTESIAN_POINT('',(-2.13418830920368,-2.,13.9091883092037));
#7295=CARTESIAN_POINT('',(-2.13418830920368,-2.4,13.9091883092037));
#7296=CARTESIAN_POINT('Origin',(-1.90918830920368,-2.,13.9091883092037));
#7297=CARTESIAN_POINT('Origin',(1.90918830920368,-2.4,13.9091883092037));
#7298=CARTESIAN_POINT('',(1.68418830920368,-2.3,13.9091883092037));
#7299=CARTESIAN_POINT('Origin',(1.90918830920368,-2.3,13.9091883092037));
#7300=CARTESIAN_POINT('',(1.68418830920368,-2.,13.9091883092037));
#7301=CARTESIAN_POINT('',(1.68418830920368,-2.4,13.9091883092037));
#7302=CARTESIAN_POINT('Origin',(1.90918830920368,-2.,13.9091883092037));
#7303=CARTESIAN_POINT('Origin',(1.90918830920368,-2.4,10.0908116907963));
#7304=CARTESIAN_POINT('',(1.68418830920368,-2.3,10.0908116907963));
#7305=CARTESIAN_POINT('Origin',(1.90918830920368,-2.3,10.0908116907963));
#7306=CARTESIAN_POINT('',(1.68418830920368,-2.,10.0908116907963));
#7307=CARTESIAN_POINT('',(1.68418830920368,-2.4,10.0908116907963));
#7308=CARTESIAN_POINT('Origin',(1.90918830920368,-2.,10.0908116907963));
#7309=CARTESIAN_POINT('Origin',(0.,-2.,12.));
#7310=CARTESIAN_POINT('',(-2.34,-1.7,12.));
#7311=CARTESIAN_POINT('Origin',(0.,-1.7,12.));
#7312=CARTESIAN_POINT('',(-2.34,-2.,12.));
#7313=CARTESIAN_POINT('',(-2.34,-2.,12.));
#7314=CARTESIAN_POINT('Origin',(0.,-2.,12.));
#7315=CARTESIAN_POINT('Origin',(0.,-1.7,12.));
#7316=CARTESIAN_POINT('',(-1.9,-1.7,12.));
#7317=CARTESIAN_POINT('Origin',(0.,-1.7,12.));
#7318=CARTESIAN_POINT('Origin',(0.,-2.3,12.));
#7319=CARTESIAN_POINT('',(-1.9,-2.3,12.));
#7320=CARTESIAN_POINT('',(-1.9,-2.3,12.));
#7321=CARTESIAN_POINT('Origin',(0.,-2.3,12.));
#7322=CARTESIAN_POINT('Origin',(0.,-2.3,12.));
#7323=CARTESIAN_POINT('',(-3.,-2.,12.));
#7324=CARTESIAN_POINT('Origin',(0.,-2.,12.));
#7325=CARTESIAN_POINT('',(-3.,-2.3,12.));
#7326=CARTESIAN_POINT('',(-3.,-2.3,12.));
#7327=CARTESIAN_POINT('Origin',(0.,-2.3,12.));
#7328=CARTESIAN_POINT('Origin',(0.,-2.,12.));
#7329=CARTESIAN_POINT('Origin',(0.,-2.3,12.));
#7330=CARTESIAN_POINT('',(0.,0.,0.));
#7331=CARTESIAN_POINT('Origin',(0.0866025403784439,-0.4,-0.15));
#7332=CARTESIAN_POINT('',(0.173205080756888,-0.4,0.));
#7333=CARTESIAN_POINT('',(0.0866025403784439,-0.4,-0.15));
#7334=CARTESIAN_POINT('',(0.173205080756888,-0.4,0.));
#7335=CARTESIAN_POINT('',(0.0866025403784439,-0.64,-0.15));
#7336=CARTESIAN_POINT('',(0.0866025403784439,-0.4,-0.15));
#7337=CARTESIAN_POINT('',(0.173205080756888,-0.64,0.));
#7338=CARTESIAN_POINT('',(0.173205080756888,-0.64,0.));
#7339=CARTESIAN_POINT('',(0.173205080756888,-0.4,0.));
#7340=CARTESIAN_POINT('Origin',(-0.0866025403784438,-0.4,-0.15));
#7341=CARTESIAN_POINT('',(-0.0866025403784438,-0.4,-0.15));
#7342=CARTESIAN_POINT('',(0.0866025403784439,-0.4,-0.15));
#7343=CARTESIAN_POINT('',(-0.0866025403784438,-0.64,-0.15));
#7344=CARTESIAN_POINT('',(-0.0866025403784438,-0.4,-0.15));
#7345=CARTESIAN_POINT('',(0.0866025403784439,-0.64,-0.15));
#7346=CARTESIAN_POINT('Origin',(-0.173205080756888,-0.4,-2.77555756156289E-17));
#7347=CARTESIAN_POINT('',(-0.173205080756888,-0.4,-2.12115047744981E-17));
#7348=CARTESIAN_POINT('',(-0.0866025403784438,-0.4,-0.15));
#7349=CARTESIAN_POINT('',(-0.173205080756888,-0.64,-2.77555756156289E-17));
#7350=CARTESIAN_POINT('',(-0.173205080756888,-0.4,-2.12115047744981E-17));
#7351=CARTESIAN_POINT('',(-0.0866025403784438,-0.64,-0.15));
#7352=CARTESIAN_POINT('Origin',(-0.0866025403784439,-0.4,0.15));
#7353=CARTESIAN_POINT('',(-0.0866025403784439,-0.4,0.15));
#7354=CARTESIAN_POINT('',(-0.173205080756888,-0.4,-2.12115047744981E-17));
#7355=CARTESIAN_POINT('',(-0.0866025403784439,-0.64,0.15));
#7356=CARTESIAN_POINT('',(-0.0866025403784439,-0.4,0.15));
#7357=CARTESIAN_POINT('',(-0.173205080756888,-0.64,-2.12115047744981E-17));
#7358=CARTESIAN_POINT('Origin',(0.0866025403784439,-0.4,0.15));
#7359=CARTESIAN_POINT('',(0.0866025403784439,-0.4,0.15));
#7360=CARTESIAN_POINT('',(-0.0866025403784439,-0.4,0.15));
#7361=CARTESIAN_POINT('',(0.0866025403784439,-0.64,0.15));
#7362=CARTESIAN_POINT('',(0.0866025403784439,-0.4,0.15));
#7363=CARTESIAN_POINT('',(-0.0866025403784439,-0.64,0.15));
#7364=CARTESIAN_POINT('Origin',(0.173205080756888,-0.4,0.));
#7365=CARTESIAN_POINT('',(0.0866025403784439,-0.4,0.15));
#7366=CARTESIAN_POINT('',(0.0866025403784439,-0.64,0.15));
#7367=CARTESIAN_POINT('Origin',(0.,-0.4,-2.77555756156289E-17));
#7368=CARTESIAN_POINT('Origin',(0.,-0.64,-2.77555756156289E-17));
#7369=CARTESIAN_POINT('Origin',(0.,-1.,0.));
#7370=CARTESIAN_POINT('',(-0.1954,-1.,2.39295984553393E-17));
#7371=CARTESIAN_POINT('Origin',(0.,-1.,0.));
#7372=CARTESIAN_POINT('Origin',(0.3,0.4,0.));
#7373=CARTESIAN_POINT('',(-0.3,0.4,-3.67394039744206E-17));
#7374=CARTESIAN_POINT('Origin',(0.,0.4,0.));
#7375=CARTESIAN_POINT('Origin',(0.,0.375,0.));
#7376=CARTESIAN_POINT('',(-0.35,0.35,-4.28626379701573E-17));
#7377=CARTESIAN_POINT('Origin',(0.,0.35,0.));
#7378=CARTESIAN_POINT('',(-0.325,0.375,-3.9801020972289E-17));
#7379=CARTESIAN_POINT('Origin',(0.,0.19,0.));
#7380=CARTESIAN_POINT('',(-0.35,0.03,-4.28626379701574E-17));
#7381=CARTESIAN_POINT('Origin',(0.,0.03,0.));
#7382=CARTESIAN_POINT('',(-0.35,0.19,-4.28626379701574E-17));
#7383=CARTESIAN_POINT('Origin',(0.,0.0149999999999999,0.));
#7384=CARTESIAN_POINT('',(-0.32,-3.29597460435593E-17,-3.91886975727153E-17));
#7385=CARTESIAN_POINT('Origin',(0.,0.,0.));
#7386=CARTESIAN_POINT('',(-0.335,0.0149999999999999,-4.10256677714363E-17));
#7387=CARTESIAN_POINT('Origin',(0.22,0.,0.));
#7388=CARTESIAN_POINT('',(-0.22,-6.93889390390723E-18,-2.69422295812418E-17));
#7389=CARTESIAN_POINT('Origin',(0.,0.,0.));
#7390=CARTESIAN_POINT('Origin',(0.,-0.02,0.));
#7391=CARTESIAN_POINT('',(-0.1954,-0.0492,2.39295984553393E-17));
#7392=CARTESIAN_POINT('Origin',(0.,-0.0492,0.));
#7393=CARTESIAN_POINT('',(-0.21,-0.02,-2.57175827820944E-17));
#7394=CARTESIAN_POINT('Origin',(0.,-0.8,0.));
#7395=CARTESIAN_POINT('',(-0.1954,-0.8,-2.39295984553393E-17));
#7396=CARTESIAN_POINT('',(0.,0.,0.));
#7397=CARTESIAN_POINT('',(0.,0.,0.));
#7398=CARTESIAN_POINT('',(0.,-1.,12.));
#7399=CARTESIAN_POINT('',(0.,1.,12.));
#7400=CARTESIAN_POINT('',(0.,0.,0.));
#7401=CARTESIAN_POINT('',(0.,0.,0.));
#7402=CARTESIAN_POINT('',(1.90918830920368,-2.3,13.9091883092037));
#7403=CARTESIAN_POINT('',(-1.90918830920368,-2.3,13.9091883092037));
#7404=CARTESIAN_POINT('',(-1.90918830920368,-2.3,10.0908116907963));
#7405=CARTESIAN_POINT('',(1.90918830920368,-2.3,10.0908116907963));
#7406=CARTESIAN_POINT('',(1.90918830920368,2.3,13.9091883092037));
#7407=CARTESIAN_POINT('',(-1.90918830920368,2.3,13.9091883092037));
#7408=CARTESIAN_POINT('',(-1.90918830920368,2.3,10.0908116907963));
#7409=CARTESIAN_POINT('',(1.90918830920368,2.3,10.0908116907963));
#7410=CARTESIAN_POINT('',(0.,0.,0.));
#7411=CARTESIAN_POINT('',(0.,0.,0.));
#7412=CARTESIAN_POINT('Origin',(0.,0.,4.48));
#7413=CARTESIAN_POINT('',(-1.3,-1.59204083889156E-16,4.48));
#7414=CARTESIAN_POINT('Origin',(0.,0.,4.48));
#7415=CARTESIAN_POINT('',(-0.8,-9.79717439317883E-17,4.48));
#7416=CARTESIAN_POINT('Origin',(0.,0.,4.48));
#7417=CARTESIAN_POINT('Origin',(0.,0.,3.88));
#7418=CARTESIAN_POINT('',(-1.3,-1.59204083889156E-16,3.88));
#7419=CARTESIAN_POINT('Origin',(0.,0.,3.88));
#7420=CARTESIAN_POINT('',(-0.8,9.79717439317883E-17,3.88));
#7421=CARTESIAN_POINT('Origin',(0.,0.,3.88));
#7422=CARTESIAN_POINT('Origin',(0.,0.,3.88));
#7423=CARTESIAN_POINT('',(-1.3,-1.59204083889156E-16,3.88));
#7424=CARTESIAN_POINT('Origin',(0.,0.,3.));
#7425=CARTESIAN_POINT('',(-0.8,-9.79717439317883E-17,3.5));
#7426=CARTESIAN_POINT('',(-0.8,-9.79717439317883E-17,3.));
#7427=CARTESIAN_POINT('',(0.,-0.8,3.5));
#7428=CARTESIAN_POINT('Origin',(0.,0.,3.5));
#7429=CARTESIAN_POINT('',(0.,0.8,3.5));
#7430=CARTESIAN_POINT('Origin',(0.,0.,3.5));
#7431=CARTESIAN_POINT('Origin',(0.,0.,3.5));
#7432=CARTESIAN_POINT('Origin',(0.,0.,3.));
#7433=CARTESIAN_POINT('',(-0.8,-9.79717439317883E-17,6.5));
#7434=CARTESIAN_POINT('Origin',(0.,0.,6.5));
#7435=CARTESIAN_POINT('',(-0.8,-9.79717439317883E-17,3.));
#7436=CARTESIAN_POINT('Origin',(0.,0.,6.5));
#7437=CARTESIAN_POINT('Origin',(-1.,-0.8,3.5));
#7438=CARTESIAN_POINT('',(1.,-0.8,3.5));
#7439=CARTESIAN_POINT('',(1.,-0.8,3.5));
#7440=CARTESIAN_POINT('',(1.,0.8,3.5));
#7441=CARTESIAN_POINT('',(1.,-0.8,3.5));
#7442=CARTESIAN_POINT('',(1.,0.8,3.5));
#7443=CARTESIAN_POINT('Origin',(-1.,-0.8,3.5));
#7444=CARTESIAN_POINT('',(-1.,0.8,3.5));
#7445=CARTESIAN_POINT('',(1.,0.8,3.5));
#7446=CARTESIAN_POINT('',(-1.,-0.8,3.5));
#7447=CARTESIAN_POINT('',(-1.,-0.8,3.5));
#7448=CARTESIAN_POINT('',(1.,-0.8,3.5));
#7449=CARTESIAN_POINT('Origin',(-1.,-0.8,0.));
#7450=CARTESIAN_POINT('',(-1.,-0.8,1.80277563773199));
#7451=CARTESIAN_POINT('',(-1.,0.8,1.80277563773199));
#7452=CARTESIAN_POINT('',(-1.,-0.8,1.80277563773199));
#7453=CARTESIAN_POINT('',(-1.,-0.8,3.5));
#7454=CARTESIAN_POINT('',(-1.,0.8,3.5));
#7455=CARTESIAN_POINT('Origin',(1.,-0.8,0.));
#7456=CARTESIAN_POINT('',(0.,0.8,0.));
#7457=CARTESIAN_POINT('',(0.,-0.8,0.));
#7458=CARTESIAN_POINT('',(0.,-0.8,0.));
#7459=CARTESIAN_POINT('',(1.,0.8,0.));
#7460=CARTESIAN_POINT('',(-1.,0.8,0.));
#7461=CARTESIAN_POINT('',(1.,-0.8,0.));
#7462=CARTESIAN_POINT('',(1.,-0.8,0.));
#7463=CARTESIAN_POINT('',(-1.,-0.8,0.));
#7464=CARTESIAN_POINT('Origin',(2.,0.8,0.));
#7465=CARTESIAN_POINT('',(1.,0.8,0.));
#7466=CARTESIAN_POINT('',(4.,0.8,0.));
#7467=CARTESIAN_POINT('Origin',(2.,0.8,0.));
#7468=CARTESIAN_POINT('',(5.5,0.8,0.));
#7469=CARTESIAN_POINT('',(4.,0.8,0.));
#7470=CARTESIAN_POINT('Origin',(2.,0.8,0.));
#7471=CARTESIAN_POINT('Origin',(2.,-0.8,0.));
#7472=CARTESIAN_POINT('',(4.,-0.8,0.));
#7473=CARTESIAN_POINT('Origin',(2.,-0.8,0.));
#7474=CARTESIAN_POINT('',(4.,-0.8,0.));
#7475=CARTESIAN_POINT('Origin',(2.,-0.8,0.));
#7476=CARTESIAN_POINT('',(1.,-0.8,0.));
#7477=CARTESIAN_POINT('',(5.5,-0.8,0.));
#7478=CARTESIAN_POINT('Origin',(2.,-0.8,0.));
#7479=CARTESIAN_POINT('',(4.,-0.8,0.));
#7480=CARTESIAN_POINT('Origin',(1.,-0.9,0.));
#7481=CARTESIAN_POINT('Origin',(6.,-0.9,0.));
#7482=CARTESIAN_POINT('',(5.5,-0.8,0.));
#7483=CARTESIAN_POINT('Origin',(2.,-0.8,0.));
#7484=CARTESIAN_POINT('',(0.,0.,0.));
#7485=CARTESIAN_POINT('Origin',(0.,0.,5.5));
#7486=CARTESIAN_POINT('',(-0.81,-9.91963907309356E-17,5.7));
#7487=CARTESIAN_POINT('Origin',(0.,0.,5.7));
#7488=CARTESIAN_POINT('',(-0.81,-9.91963907309356E-17,5.5));
#7489=CARTESIAN_POINT('',(-0.81,-9.91963907309356E-17,5.5));
#7490=CARTESIAN_POINT('Origin',(0.,0.,5.5));
#7491=CARTESIAN_POINT('Origin',(0.,0.,5.5));
#7492=CARTESIAN_POINT('',(-1.5,-1.83697019872103E-16,5.7));
#7493=CARTESIAN_POINT('Origin',(0.,0.,5.7));
#7494=CARTESIAN_POINT('',(-1.5,-1.83697019872103E-16,5.5));
#7495=CARTESIAN_POINT('',(-1.5,-1.83697019872103E-16,5.5));
#7496=CARTESIAN_POINT('Origin',(0.,0.,5.5));
#7497=CARTESIAN_POINT('Origin',(0.,0.,5.7));
#7498=CARTESIAN_POINT('Origin',(0.,0.,5.5));
#7499=CARTESIAN_POINT('',(0.,0.,0.));
#7500=CARTESIAN_POINT('Origin',(0.,0.,5.6));
#7501=CARTESIAN_POINT('',(-0.7,-8.57252759403147E-17,5.7));
#7502=CARTESIAN_POINT('Origin',(0.,0.,5.7));
#7503=CARTESIAN_POINT('',(-0.7,8.57252759403147E-17,6.5));
#7504=CARTESIAN_POINT('',(-0.7,-8.57252759403147E-17,5.6));
#7505=CARTESIAN_POINT('Origin',(0.,0.,6.5));
#7506=CARTESIAN_POINT('Origin',(-0.692820323027552,-1.2,5.7));
#7507=CARTESIAN_POINT('',(-0.692820323027552,-1.2,5.7));
#7508=CARTESIAN_POINT('',(0.692820323027551,-1.2,5.7));
#7509=CARTESIAN_POINT('',(-0.692820323027552,-1.2,5.7));
#7510=CARTESIAN_POINT('',(0.692820323027551,-1.2,6.5));
#7511=CARTESIAN_POINT('',(0.692820323027551,-1.2,5.7));
#7512=CARTESIAN_POINT('',(-0.692820323027552,-1.2,6.5));
#7513=CARTESIAN_POINT('',(-0.692820323027552,-1.2,6.5));
#7514=CARTESIAN_POINT('',(-0.692820323027552,-1.2,5.7));
#7515=CARTESIAN_POINT('Origin',(-1.3856406460551,1.69692038195985E-16,5.7));
#7516=CARTESIAN_POINT('',(-1.3856406460551,1.69692038195985E-16,5.7));
#7517=CARTESIAN_POINT('',(-1.3856406460551,1.69692038195985E-16,5.7));
#7518=CARTESIAN_POINT('',(-1.3856406460551,2.22044604925031E-16,6.5));
#7519=CARTESIAN_POINT('',(-1.3856406460551,1.69692038195985E-16,6.5));
#7520=CARTESIAN_POINT('',(-1.3856406460551,1.69692038195985E-16,5.7));
#7521=CARTESIAN_POINT('Origin',(-0.692820323027551,1.2,5.7));
#7522=CARTESIAN_POINT('',(-0.692820323027551,1.2,5.7));
#7523=CARTESIAN_POINT('',(-0.692820323027551,1.2,5.7));
#7524=CARTESIAN_POINT('',(-0.692820323027551,1.2,6.5));
#7525=CARTESIAN_POINT('',(-0.692820323027551,1.2,6.5));
#7526=CARTESIAN_POINT('',(-0.692820323027551,1.2,5.7));
#7527=CARTESIAN_POINT('Origin',(0.692820323027551,1.2,5.7));
#7528=CARTESIAN_POINT('',(0.692820323027551,1.2,5.7));
#7529=CARTESIAN_POINT('',(0.692820323027551,1.2,5.7));
#7530=CARTESIAN_POINT('',(0.692820323027551,1.2,6.5));
#7531=CARTESIAN_POINT('',(0.692820323027551,1.2,6.5));
#7532=CARTESIAN_POINT('',(0.692820323027551,1.2,5.7));
#7533=CARTESIAN_POINT('Origin',(1.3856406460551,0.,5.7));
#7534=CARTESIAN_POINT('',(1.3856406460551,0.,5.7));
#7535=CARTESIAN_POINT('',(1.3856406460551,0.,5.7));
#7536=CARTESIAN_POINT('',(1.3856406460551,0.,6.5));
#7537=CARTESIAN_POINT('',(1.3856406460551,0.,6.5));
#7538=CARTESIAN_POINT('',(1.3856406460551,0.,5.7));
#7539=CARTESIAN_POINT('Origin',(0.692820323027551,-1.2,5.7));
#7540=CARTESIAN_POINT('',(0.692820323027551,-1.2,5.7));
#7541=CARTESIAN_POINT('',(0.692820323027551,-1.2,6.5));
#7542=CARTESIAN_POINT('Origin',(0.,2.22044604925031E-16,6.5));
#7543=CARTESIAN_POINT('Origin',(0.,2.22044604925031E-16,5.7));
#7544=CARTESIAN_POINT('',(0.,0.,0.));
#7545=CARTESIAN_POINT('',(0.,0.,0.));
#7546=CARTESIAN_POINT('',(0.,0.,0.));
#7547=CARTESIAN_POINT('',(0.,0.,0.));
#7548=CARTESIAN_POINT('',(0.,0.,0.));
#7549=CARTESIAN_POINT('',(0.,0.,0.));
#7550=UNCERTAINTY_MEASURE_WITH_UNIT(LENGTH_MEASURE(0.001),#7610,
'DISTANCE_ACCURACY_VALUE',
'Maximum model space distance between geometric entities at asserted c
onnectivities');
#7551=UNCERTAINTY_MEASURE_WITH_UNIT(LENGTH_MEASURE(0.001),#7610,
'DISTANCE_ACCURACY_VALUE',
'Maximum model space distance between geometric entities at asserted c
onnectivities');
#7552=UNCERTAINTY_MEASURE_WITH_UNIT(LENGTH_MEASURE(0.001),#7610,
'DISTANCE_ACCURACY_VALUE',
'Maximum model space distance between geometric entities at asserted c
onnectivities');
#7553=UNCERTAINTY_MEASURE_WITH_UNIT(LENGTH_MEASURE(0.001),#7610,
'DISTANCE_ACCURACY_VALUE',
'Maximum model space distance between geometric entities at asserted c
onnectivities');
#7554=UNCERTAINTY_MEASURE_WITH_UNIT(LENGTH_MEASURE(0.001),#7610,
'DISTANCE_ACCURACY_VALUE',
'Maximum model space distance between geometric entities at asserted c
onnectivities');
#7555=UNCERTAINTY_MEASURE_WITH_UNIT(LENGTH_MEASURE(0.001),#7610,
'DISTANCE_ACCURACY_VALUE',
'Maximum model space distance between geometric entities at asserted c
onnectivities');
#7556=UNCERTAINTY_MEASURE_WITH_UNIT(LENGTH_MEASURE(0.001),#7610,
'DISTANCE_ACCURACY_VALUE',
'Maximum model space distance between geometric entities at asserted c
onnectivities');
#7557=UNCERTAINTY_MEASURE_WITH_UNIT(LENGTH_MEASURE(0.001),#7610,
'DISTANCE_ACCURACY_VALUE',
'Maximum model space distance between geometric entities at asserted c
onnectivities');
#7558=UNCERTAINTY_MEASURE_WITH_UNIT(LENGTH_MEASURE(0.001),#7610,
'DISTANCE_ACCURACY_VALUE',
'Maximum model space distance between geometric entities at asserted c
onnectivities');
#7559=UNCERTAINTY_MEASURE_WITH_UNIT(LENGTH_MEASURE(0.001),#7610,
'DISTANCE_ACCURACY_VALUE',
'Maximum model space distance between geometric entities at asserted c
onnectivities');
#7560=UNCERTAINTY_MEASURE_WITH_UNIT(LENGTH_MEASURE(0.001),#7610,
'DISTANCE_ACCURACY_VALUE',
'Maximum model space distance between geometric entities at asserted c
onnectivities');
#7561=UNCERTAINTY_MEASURE_WITH_UNIT(LENGTH_MEASURE(0.001),#7610,
'DISTANCE_ACCURACY_VALUE',
'Maximum model space distance between geometric entities at asserted c
onnectivities');
#7562=UNCERTAINTY_MEASURE_WITH_UNIT(LENGTH_MEASURE(0.001),#7610,
'DISTANCE_ACCURACY_VALUE',
'Maximum model space distance between geometric entities at asserted c
onnectivities');
#7563=UNCERTAINTY_MEASURE_WITH_UNIT(LENGTH_MEASURE(0.001),#7610,
'DISTANCE_ACCURACY_VALUE',
'Maximum model space distance between geometric entities at asserted c
onnectivities');
#7564=UNCERTAINTY_MEASURE_WITH_UNIT(LENGTH_MEASURE(0.001),#7610,
'DISTANCE_ACCURACY_VALUE',
'Maximum model space distance between geometric entities at asserted c
onnectivities');
#7565=UNCERTAINTY_MEASURE_WITH_UNIT(LENGTH_MEASURE(0.001),#7610,
'DISTANCE_ACCURACY_VALUE',
'Maximum model space distance between geometric entities at asserted c
onnectivities');
#7566=UNCERTAINTY_MEASURE_WITH_UNIT(LENGTH_MEASURE(0.001),#7610,
'DISTANCE_ACCURACY_VALUE',
'Maximum model space distance between geometric entities at asserted c
onnectivities');
#7567=UNCERTAINTY_MEASURE_WITH_UNIT(LENGTH_MEASURE(0.001),#7610,
'DISTANCE_ACCURACY_VALUE',
'Maximum model space distance between geometric entities at asserted c
onnectivities');
#7568=UNCERTAINTY_MEASURE_WITH_UNIT(LENGTH_MEASURE(0.001),#7610,
'DISTANCE_ACCURACY_VALUE',
'Maximum model space distance between geometric entities at asserted c
onnectivities');
#7569=UNCERTAINTY_MEASURE_WITH_UNIT(LENGTH_MEASURE(0.001),#7610,
'DISTANCE_ACCURACY_VALUE',
'Maximum model space distance between geometric entities at asserted c
onnectivities');
#7570=UNCERTAINTY_MEASURE_WITH_UNIT(LENGTH_MEASURE(0.001),#7610,
'DISTANCE_ACCURACY_VALUE',
'Maximum model space distance between geometric entities at asserted c
onnectivities');
#7571=UNCERTAINTY_MEASURE_WITH_UNIT(LENGTH_MEASURE(0.001),#7610,
'DISTANCE_ACCURACY_VALUE',
'Maximum model space distance between geometric entities at asserted c
onnectivities');
#7572=UNCERTAINTY_MEASURE_WITH_UNIT(LENGTH_MEASURE(0.001),#7610,
'DISTANCE_ACCURACY_VALUE',
'Maximum model space distance between geometric entities at asserted c
onnectivities');
#7573=UNCERTAINTY_MEASURE_WITH_UNIT(LENGTH_MEASURE(0.001),#7610,
'DISTANCE_ACCURACY_VALUE',
'Maximum model space distance between geometric entities at asserted c
onnectivities');
#7574=UNCERTAINTY_MEASURE_WITH_UNIT(LENGTH_MEASURE(0.001),#7610,
'DISTANCE_ACCURACY_VALUE',
'Maximum model space distance between geometric entities at asserted c
onnectivities');
#7575=UNCERTAINTY_MEASURE_WITH_UNIT(LENGTH_MEASURE(0.001),#7610,
'DISTANCE_ACCURACY_VALUE',
'Maximum model space distance between geometric entities at asserted c
onnectivities');
#7576=UNCERTAINTY_MEASURE_WITH_UNIT(LENGTH_MEASURE(0.001),#7610,
'DISTANCE_ACCURACY_VALUE',
'Maximum model space distance between geometric entities at asserted c
onnectivities');
#7577=UNCERTAINTY_MEASURE_WITH_UNIT(LENGTH_MEASURE(0.001),#7610,
'DISTANCE_ACCURACY_VALUE',
'Maximum model space distance between geometric entities at asserted c
onnectivities');
#7578=UNCERTAINTY_MEASURE_WITH_UNIT(LENGTH_MEASURE(0.001),#7610,
'DISTANCE_ACCURACY_VALUE',
'Maximum model space distance between geometric entities at asserted c
onnectivities');
#7579=UNCERTAINTY_MEASURE_WITH_UNIT(LENGTH_MEASURE(0.001),#7610,
'DISTANCE_ACCURACY_VALUE',
'Maximum model space distance between geometric entities at asserted c
onnectivities');
#7580=(
GEOMETRIC_REPRESENTATION_CONTEXT(3)
GLOBAL_UNCERTAINTY_ASSIGNED_CONTEXT((#7550))
GLOBAL_UNIT_ASSIGNED_CONTEXT((#7610,#7612,#7613))
REPRESENTATION_CONTEXT('','3D')
);
#7581=(
GEOMETRIC_REPRESENTATION_CONTEXT(3)
GLOBAL_UNCERTAINTY_ASSIGNED_CONTEXT((#7551))
GLOBAL_UNIT_ASSIGNED_CONTEXT((#7610,#7612,#7613))
REPRESENTATION_CONTEXT('','3D')
);
#7582=(
GEOMETRIC_REPRESENTATION_CONTEXT(3)
GLOBAL_UNCERTAINTY_ASSIGNED_CONTEXT((#7552))
GLOBAL_UNIT_ASSIGNED_CONTEXT((#7610,#7612,#7613))
REPRESENTATION_CONTEXT('','3D')
);
#7583=(
GEOMETRIC_REPRESENTATION_CONTEXT(3)
GLOBAL_UNCERTAINTY_ASSIGNED_CONTEXT((#7553))
GLOBAL_UNIT_ASSIGNED_CONTEXT((#7610,#7612,#7613))
REPRESENTATION_CONTEXT('','3D')
);
#7584=(
GEOMETRIC_REPRESENTATION_CONTEXT(3)
GLOBAL_UNCERTAINTY_ASSIGNED_CONTEXT((#7554))
GLOBAL_UNIT_ASSIGNED_CONTEXT((#7610,#7612,#7613))
REPRESENTATION_CONTEXT('','3D')
);
#7585=(
GEOMETRIC_REPRESENTATION_CONTEXT(3)
GLOBAL_UNCERTAINTY_ASSIGNED_CONTEXT((#7555))
GLOBAL_UNIT_ASSIGNED_CONTEXT((#7610,#7612,#7613))
REPRESENTATION_CONTEXT('','3D')
);
#7586=(
GEOMETRIC_REPRESENTATION_CONTEXT(3)
GLOBAL_UNCERTAINTY_ASSIGNED_CONTEXT((#7556))
GLOBAL_UNIT_ASSIGNED_CONTEXT((#7610,#7612,#7613))
REPRESENTATION_CONTEXT('','3D')
);
#7587=(
GEOMETRIC_REPRESENTATION_CONTEXT(3)
GLOBAL_UNCERTAINTY_ASSIGNED_CONTEXT((#7557))
GLOBAL_UNIT_ASSIGNED_CONTEXT((#7610,#7612,#7613))
REPRESENTATION_CONTEXT('','3D')
);
#7588=(
GEOMETRIC_REPRESENTATION_CONTEXT(3)
GLOBAL_UNCERTAINTY_ASSIGNED_CONTEXT((#7558))
GLOBAL_UNIT_ASSIGNED_CONTEXT((#7610,#7612,#7613))
REPRESENTATION_CONTEXT('','3D')
);
#7589=(
GEOMETRIC_REPRESENTATION_CONTEXT(3)
GLOBAL_UNCERTAINTY_ASSIGNED_CONTEXT((#7559))
GLOBAL_UNIT_ASSIGNED_CONTEXT((#7610,#7612,#7613))
REPRESENTATION_CONTEXT('','3D')
);
#7590=(
GEOMETRIC_REPRESENTATION_CONTEXT(3)
GLOBAL_UNCERTAINTY_ASSIGNED_CONTEXT((#7560))
GLOBAL_UNIT_ASSIGNED_CONTEXT((#7610,#7612,#7613))
REPRESENTATION_CONTEXT('','3D')
);
#7591=(
GEOMETRIC_REPRESENTATION_CONTEXT(3)
GLOBAL_UNCERTAINTY_ASSIGNED_CONTEXT((#7561))
GLOBAL_UNIT_ASSIGNED_CONTEXT((#7610,#7612,#7613))
REPRESENTATION_CONTEXT('','3D')
);
#7592=(
GEOMETRIC_REPRESENTATION_CONTEXT(3)
GLOBAL_UNCERTAINTY_ASSIGNED_CONTEXT((#7562))
GLOBAL_UNIT_ASSIGNED_CONTEXT((#7610,#7612,#7613))
REPRESENTATION_CONTEXT('','3D')
);
#7593=(
GEOMETRIC_REPRESENTATION_CONTEXT(3)
GLOBAL_UNCERTAINTY_ASSIGNED_CONTEXT((#7563))
GLOBAL_UNIT_ASSIGNED_CONTEXT((#7610,#7612,#7613))
REPRESENTATION_CONTEXT('','3D')
);
#7594=(
GEOMETRIC_REPRESENTATION_CONTEXT(3)
GLOBAL_UNCERTAINTY_ASSIGNED_CONTEXT((#7564))
GLOBAL_UNIT_ASSIGNED_CONTEXT((#7610,#7612,#7613))
REPRESENTATION_CONTEXT('','3D')
);
#7595=(
GEOMETRIC_REPRESENTATION_CONTEXT(3)
GLOBAL_UNCERTAINTY_ASSIGNED_CONTEXT((#7565))
GLOBAL_UNIT_ASSIGNED_CONTEXT((#7610,#7612,#7613))
REPRESENTATION_CONTEXT('','3D')
);
#7596=(
GEOMETRIC_REPRESENTATION_CONTEXT(3)
GLOBAL_UNCERTAINTY_ASSIGNED_CONTEXT((#7566))
GLOBAL_UNIT_ASSIGNED_CONTEXT((#7610,#7612,#7613))
REPRESENTATION_CONTEXT('','3D')
);
#7597=(
GEOMETRIC_REPRESENTATION_CONTEXT(3)
GLOBAL_UNCERTAINTY_ASSIGNED_CONTEXT((#7567))
GLOBAL_UNIT_ASSIGNED_CONTEXT((#7610,#7612,#7613))
REPRESENTATION_CONTEXT('','3D')
);
#7598=(
GEOMETRIC_REPRESENTATION_CONTEXT(3)
GLOBAL_UNCERTAINTY_ASSIGNED_CONTEXT((#7568))
GLOBAL_UNIT_ASSIGNED_CONTEXT((#7610,#7612,#7613))
REPRESENTATION_CONTEXT('','3D')
);
#7599=(
GEOMETRIC_REPRESENTATION_CONTEXT(3)
GLOBAL_UNCERTAINTY_ASSIGNED_CONTEXT((#7569))
GLOBAL_UNIT_ASSIGNED_CONTEXT((#7610,#7612,#7613))
REPRESENTATION_CONTEXT('','3D')
);
#7600=(
GEOMETRIC_REPRESENTATION_CONTEXT(3)
GLOBAL_UNCERTAINTY_ASSIGNED_CONTEXT((#7570))
GLOBAL_UNIT_ASSIGNED_CONTEXT((#7610,#7612,#7613))
REPRESENTATION_CONTEXT('','3D')
);
#7601=(
GEOMETRIC_REPRESENTATION_CONTEXT(3)
GLOBAL_UNCERTAINTY_ASSIGNED_CONTEXT((#7571))
GLOBAL_UNIT_ASSIGNED_CONTEXT((#7610,#7612,#7613))
REPRESENTATION_CONTEXT('','3D')
);
#7602=(
GEOMETRIC_REPRESENTATION_CONTEXT(3)
GLOBAL_UNCERTAINTY_ASSIGNED_CONTEXT((#7572))
GLOBAL_UNIT_ASSIGNED_CONTEXT((#7610,#7612,#7613))
REPRESENTATION_CONTEXT('','3D')
);
#7603=(
GEOMETRIC_REPRESENTATION_CONTEXT(3)
GLOBAL_UNCERTAINTY_ASSIGNED_CONTEXT((#7573))
GLOBAL_UNIT_ASSIGNED_CONTEXT((#7610,#7612,#7613))
REPRESENTATION_CONTEXT('','3D')
);
#7604=(
GEOMETRIC_REPRESENTATION_CONTEXT(3)
GLOBAL_UNCERTAINTY_ASSIGNED_CONTEXT((#7574))
GLOBAL_UNIT_ASSIGNED_CONTEXT((#7610,#7612,#7613))
REPRESENTATION_CONTEXT('','3D')
);
#7605=(
GEOMETRIC_REPRESENTATION_CONTEXT(3)
GLOBAL_UNCERTAINTY_ASSIGNED_CONTEXT((#7575))
GLOBAL_UNIT_ASSIGNED_CONTEXT((#7610,#7612,#7613))
REPRESENTATION_CONTEXT('','3D')
);
#7606=(
GEOMETRIC_REPRESENTATION_CONTEXT(3)
GLOBAL_UNCERTAINTY_ASSIGNED_CONTEXT((#7576))
GLOBAL_UNIT_ASSIGNED_CONTEXT((#7610,#7612,#7613))
REPRESENTATION_CONTEXT('','3D')
);
#7607=(
GEOMETRIC_REPRESENTATION_CONTEXT(3)
GLOBAL_UNCERTAINTY_ASSIGNED_CONTEXT((#7577))
GLOBAL_UNIT_ASSIGNED_CONTEXT((#7610,#7612,#7613))
REPRESENTATION_CONTEXT('','3D')
);
#7608=(
GEOMETRIC_REPRESENTATION_CONTEXT(3)
GLOBAL_UNCERTAINTY_ASSIGNED_CONTEXT((#7578))
GLOBAL_UNIT_ASSIGNED_CONTEXT((#7610,#7612,#7613))
REPRESENTATION_CONTEXT('','3D')
);
#7609=(
GEOMETRIC_REPRESENTATION_CONTEXT(3)
GLOBAL_UNCERTAINTY_ASSIGNED_CONTEXT((#7579))
GLOBAL_UNIT_ASSIGNED_CONTEXT((#7610,#7612,#7613))
REPRESENTATION_CONTEXT('','3D')
);
#7610=(
LENGTH_UNIT()
NAMED_UNIT(*)
SI_UNIT(.CENTI.,.METRE.)
);
#7611=(
LENGTH_UNIT()
NAMED_UNIT(*)
SI_UNIT($,.METRE.)
);
#7612=(
NAMED_UNIT(*)
PLANE_ANGLE_UNIT()
SI_UNIT($,.RADIAN.)
);
#7613=(
NAMED_UNIT(*)
SI_UNIT($,.STERADIAN.)
SOLID_ANGLE_UNIT()
);
#7614=SHAPE_DEFINITION_REPRESENTATION(#7643,#7720);
#7615=SHAPE_DEFINITION_REPRESENTATION(#7644,#7721);
#7616=SHAPE_DEFINITION_REPRESENTATION(#7645,#7722);
#7617=SHAPE_DEFINITION_REPRESENTATION(#7646,#7723);
#7618=SHAPE_DEFINITION_REPRESENTATION(#7647,#7724);
#7619=SHAPE_DEFINITION_REPRESENTATION(#7648,#7725);
#7620=SHAPE_DEFINITION_REPRESENTATION(#7649,#7726);
#7621=SHAPE_DEFINITION_REPRESENTATION(#7650,#7727);
#7622=SHAPE_DEFINITION_REPRESENTATION(#7651,#7728);
#7623=SHAPE_DEFINITION_REPRESENTATION(#7652,#7729);
#7624=SHAPE_DEFINITION_REPRESENTATION(#7653,#7730);
#7625=SHAPE_DEFINITION_REPRESENTATION(#7654,#7731);
#7626=SHAPE_DEFINITION_REPRESENTATION(#7655,#7732);
#7627=SHAPE_DEFINITION_REPRESENTATION(#7656,#7733);
#7628=SHAPE_DEFINITION_REPRESENTATION(#7680,#7734);
#7629=SHAPE_DEFINITION_REPRESENTATION(#7681,#7735);
#7630=SHAPE_DEFINITION_REPRESENTATION(#7682,#7736);
#7631=SHAPE_DEFINITION_REPRESENTATION(#7683,#7737);
#7632=SHAPE_DEFINITION_REPRESENTATION(#7684,#7738);
#7633=SHAPE_DEFINITION_REPRESENTATION(#7685,#7739);
#7634=SHAPE_DEFINITION_REPRESENTATION(#7686,#7740);
#7635=SHAPE_DEFINITION_REPRESENTATION(#7687,#7741);
#7636=SHAPE_DEFINITION_REPRESENTATION(#7688,#7742);
#7637=SHAPE_DEFINITION_REPRESENTATION(#7694,#7743);
#7638=SHAPE_DEFINITION_REPRESENTATION(#7695,#7744);
#7639=SHAPE_DEFINITION_REPRESENTATION(#7710,#7745);
#7640=SHAPE_DEFINITION_REPRESENTATION(#7711,#7746);
#7641=SHAPE_DEFINITION_REPRESENTATION(#7712,#7747);
#7642=SHAPE_DEFINITION_REPRESENTATION(#7713,#7748);
#7643=PRODUCT_DEFINITION_SHAPE('',$,#7750);
#7644=PRODUCT_DEFINITION_SHAPE('',$,#7751);
#7645=PRODUCT_DEFINITION_SHAPE('',$,#7752);
#7646=PRODUCT_DEFINITION_SHAPE('',$,#7753);
#7647=PRODUCT_DEFINITION_SHAPE('',$,#7754);
#7648=PRODUCT_DEFINITION_SHAPE('',$,#7755);
#7649=PRODUCT_DEFINITION_SHAPE('',$,#7756);
#7650=PRODUCT_DEFINITION_SHAPE('',$,#7757);
#7651=PRODUCT_DEFINITION_SHAPE('',$,#7758);
#7652=PRODUCT_DEFINITION_SHAPE('',$,#7759);
#7653=PRODUCT_DEFINITION_SHAPE('',$,#7760);
#7654=PRODUCT_DEFINITION_SHAPE('',$,#7761);
#7655=PRODUCT_DEFINITION_SHAPE('',$,#7762);
#7656=PRODUCT_DEFINITION_SHAPE('',$,#7763);
#7657=PRODUCT_DEFINITION_SHAPE($,$,#191);
#7658=PRODUCT_DEFINITION_SHAPE($,$,#192);
#7659=PRODUCT_DEFINITION_SHAPE($,$,#193);
#7660=PRODUCT_DEFINITION_SHAPE($,$,#194);
#7661=PRODUCT_DEFINITION_SHAPE($,$,#195);
#7662=PRODUCT_DEFINITION_SHAPE($,$,#196);
#7663=PRODUCT_DEFINITION_SHAPE($,$,#197);
#7664=PRODUCT_DEFINITION_SHAPE($,$,#198);
#7665=PRODUCT_DEFINITION_SHAPE($,$,#199);
#7666=PRODUCT_DEFINITION_SHAPE($,$,#200);
#7667=PRODUCT_DEFINITION_SHAPE($,$,#201);
#7668=PRODUCT_DEFINITION_SHAPE($,$,#202);
#7669=PRODUCT_DEFINITION_SHAPE($,$,#203);
#7670=PRODUCT_DEFINITION_SHAPE($,$,#204);
#7671=PRODUCT_DEFINITION_SHAPE($,$,#205);
#7672=PRODUCT_DEFINITION_SHAPE($,$,#206);
#7673=PRODUCT_DEFINITION_SHAPE($,$,#207);
#7674=PRODUCT_DEFINITION_SHAPE($,$,#208);
#7675=PRODUCT_DEFINITION_SHAPE($,$,#209);
#7676=PRODUCT_DEFINITION_SHAPE($,$,#210);
#7677=PRODUCT_DEFINITION_SHAPE($,$,#211);
#7678=PRODUCT_DEFINITION_SHAPE($,$,#212);
#7679=PRODUCT_DEFINITION_SHAPE($,$,#213);
#7680=PRODUCT_DEFINITION_SHAPE('',$,#7764);
#7681=PRODUCT_DEFINITION_SHAPE('',$,#7765);
#7682=PRODUCT_DEFINITION_SHAPE('',$,#7766);
#7683=PRODUCT_DEFINITION_SHAPE('',$,#7767);
#7684=PRODUCT_DEFINITION_SHAPE('',$,#7768);
#7685=PRODUCT_DEFINITION_SHAPE('',$,#7769);
#7686=PRODUCT_DEFINITION_SHAPE('',$,#7770);
#7687=PRODUCT_DEFINITION_SHAPE('',$,#7771);
#7688=PRODUCT_DEFINITION_SHAPE('',$,#7772);
#7689=PRODUCT_DEFINITION_SHAPE($,$,#214);
#7690=PRODUCT_DEFINITION_SHAPE($,$,#215);
#7691=PRODUCT_DEFINITION_SHAPE($,$,#216);
#7692=PRODUCT_DEFINITION_SHAPE($,$,#217);
#7693=PRODUCT_DEFINITION_SHAPE($,$,#218);
#7694=PRODUCT_DEFINITION_SHAPE('',$,#7773);
#7695=PRODUCT_DEFINITION_SHAPE('',$,#7774);
#7696=PRODUCT_DEFINITION_SHAPE($,$,#219);
#7697=PRODUCT_DEFINITION_SHAPE($,$,#220);
#7698=PRODUCT_DEFINITION_SHAPE($,$,#221);
#7699=PRODUCT_DEFINITION_SHAPE($,$,#222);
#7700=PRODUCT_DEFINITION_SHAPE($,$,#223);
#7701=PRODUCT_DEFINITION_SHAPE($,$,#224);
#7702=PRODUCT_DEFINITION_SHAPE($,$,#225);
#7703=PRODUCT_DEFINITION_SHAPE($,$,#226);
#7704=PRODUCT_DEFINITION_SHAPE($,$,#227);
#7705=PRODUCT_DEFINITION_SHAPE($,$,#228);
#7706=PRODUCT_DEFINITION_SHAPE($,$,#229);
#7707=PRODUCT_DEFINITION_SHAPE($,$,#230);
#7708=PRODUCT_DEFINITION_SHAPE($,$,#231);
#7709=PRODUCT_DEFINITION_SHAPE($,$,#232);
#7710=PRODUCT_DEFINITION_SHAPE('',$,#7775);
#7711=PRODUCT_DEFINITION_SHAPE('',$,#7776);
#7712=PRODUCT_DEFINITION_SHAPE('',$,#7777);
#7713=PRODUCT_DEFINITION_SHAPE('',$,#7778);
#7714=PRODUCT_DEFINITION_SHAPE($,$,#233);
#7715=PRODUCT_DEFINITION_SHAPE($,$,#234);
#7716=PRODUCT_DEFINITION_SHAPE($,$,#235);
#7717=PRODUCT_DEFINITION_SHAPE($,$,#236);
#7718=PRODUCT_DEFINITION_SHAPE($,$,#237);
#7719=PRODUCT_DEFINITION_SHAPE($,$,#238);
#7720=SHAPE_REPRESENTATION('',(#4219,#4754,#4755,#4756),#7580);
#7721=SHAPE_REPRESENTATION('',(#4220,#4435,#4436,#4437,#4438,#4439,#4440,
#4441,#4442,#4443,#4444,#4445,#4446,#4447,#4448,#4449,#4450,#4451,#4452,
#4453,#4454,#4455,#4456,#4457),#7581);
#7722=SHAPE_REPRESENTATION('',(#4221),#7582);
#7723=SHAPE_REPRESENTATION('',(#4281),#7583);
#7724=SHAPE_REPRESENTATION('',(#4297),#7584);
#7725=SHAPE_REPRESENTATION('',(#4306),#7585);
#7726=SHAPE_REPRESENTATION('',(#4320),#7586);
#7727=SHAPE_REPRESENTATION('',(#4329),#7587);
#7728=SHAPE_REPRESENTATION('',(#4338),#7588);
#7729=SHAPE_REPRESENTATION('',(#4347),#7589);
#7730=SHAPE_REPRESENTATION('',(#4356),#7590);
#7731=SHAPE_REPRESENTATION('',(#4384),#7591);
#7732=SHAPE_REPRESENTATION('',(#4393),#7592);
#7733=SHAPE_REPRESENTATION('',(#4409),#7593);
#7734=SHAPE_REPRESENTATION('',(#4458,#4686,#4687,#4688,#4689,#4690,#4691,
#4692,#4693,#4694,#4695,#4696,#4697,#4698,#4699),#7594);
#7735=SHAPE_REPRESENTATION('',(#4459),#7595);
#7736=SHAPE_REPRESENTATION('',(#4494),#7596);
#7737=SHAPE_REPRESENTATION('',(#4503,#4632,#4633,#4634,#4635,#4636),#7597);
#7738=SHAPE_REPRESENTATION('',(#4504),#7598);
#7739=SHAPE_REPRESENTATION('',(#4524),#7599);
#7740=SHAPE_REPRESENTATION('',(#4544),#7600);
#7741=SHAPE_REPRESENTATION('',(#4561),#7601);
#7742=SHAPE_REPRESENTATION('',(#4615),#7602);
#7743=SHAPE_REPRESENTATION('',(#4637),#7603);
#7744=SHAPE_REPRESENTATION('',(#4662),#7604);
#7745=SHAPE_REPRESENTATION('',(#4700,#4751,#4752,#4753),#7605);
#7746=SHAPE_REPRESENTATION('',(#4701),#7606);
#7747=SHAPE_REPRESENTATION('',(#4730),#7607);
#7748=SHAPE_REPRESENTATION('',(#4739),#7608);
#7749=PRODUCT_DEFINITION_CONTEXT('part definition',#7838,'design');
#7750=PRODUCT_DEFINITION('PAT-057','PAT-057',#7779,
#7749);
#7751=PRODUCT_DEFINITION('Side plates and axle','Side plates and axle',
#7780,#7749);
#7752=PRODUCT_DEFINITION('Side plate','Side plate',#7781,#7749);
#7753=PRODUCT_DEFINITION('Hook bridge','Hook bridge',#7782,#7749);
#7754=PRODUCT_DEFINITION('Eye axle sleeve','Eye axle sleeve',#7783,#7749);
#7755=PRODUCT_DEFINITION('Sheave axle','Sheave axle',#7784,#7749);
#7756=PRODUCT_DEFINITION('Axle keeper','Axle keeper',#7785,#7749);
#7757=PRODUCT_DEFINITION('Central inner-race spacer',
'Central inner-race spacer',#7786,#7749);
#7758=PRODUCT_DEFINITION('Hook bushing','Hook bushing',#7787,#7749);
#7759=PRODUCT_DEFINITION('Outer inner-race spacer',
'Outer inner-race spacer',#7788,#7749);
#7760=PRODUCT_DEFINITION('M8x75 cross bolt','M8x75 cross bolt',#7789,#7749);
#7761=PRODUCT_DEFINITION('Flat Washer - M8','Flat Washer - M8',#7790,#7749);
#7762=PRODUCT_DEFINITION('Hex Nut - M8','Hex Nut - M8',#7791,#7749);
#7763=PRODUCT_DEFINITION('Cap Screw - M8x30','Cap Screw - M8x30',#7792,
#7749);
#7764=PRODUCT_DEFINITION('Bearing sheave','Bearing sheave',#7793,#7749);
#7765=PRODUCT_DEFINITION('Sheave','Sheave',#7794,#7749);
#7766=PRODUCT_DEFINITION('Outer race spacer','Outer race spacer',#7795,
#7749);
#7767=PRODUCT_DEFINITION('Sealed Ball Bearing - 20 x 47 x 14 mm',
'Sealed Ball Bearing - 20 x 47 x 14 mm',#7796,#7749);
#7768=PRODUCT_DEFINITION('Inner ring','Inner ring',#7797,#7749);
#7769=PRODUCT_DEFINITION('Outer ring','Outer ring',#7798,#7749);
#7770=PRODUCT_DEFINITION('Balls','Balls',#7799,#7749);
#7771=PRODUCT_DEFINITION('Cage','Cage',#7800,#7749);
#7772=PRODUCT_DEFINITION('Seals 2RS','Seals 2RS',#7801,#7749);
#7773=PRODUCT_DEFINITION('Sheave cap','Sheave cap',#7802,#7749);
#7774=PRODUCT_DEFINITION('M4x10 Cap Screw','M4x10 Cap Screw',#7803,#7749);
#7775=PRODUCT_DEFINITION('Swivelling hook','Swivelling hook',#7804,#7749);
#7776=PRODUCT_DEFINITION('Hook','Hook',#7805,#7749);
#7777=PRODUCT_DEFINITION('Swivel thrust washer','Swivel thrust washer',
#7806,#7749);
#7778=PRODUCT_DEFINITION('M16 hook retaining nut',
'M16 hook retaining nut',#7807,#7749);
#7779=PRODUCT_DEFINITION_FORMATION('',$,#7840);
#7780=PRODUCT_DEFINITION_FORMATION('',$,#7841);
#7781=PRODUCT_DEFINITION_FORMATION('',$,#7842);
#7782=PRODUCT_DEFINITION_FORMATION('',$,#7843);
#7783=PRODUCT_DEFINITION_FORMATION('',$,#7844);
#7784=PRODUCT_DEFINITION_FORMATION('',$,#7845);
#7785=PRODUCT_DEFINITION_FORMATION('',$,#7846);
#7786=PRODUCT_DEFINITION_FORMATION('',$,#7847);
#7787=PRODUCT_DEFINITION_FORMATION('',$,#7848);
#7788=PRODUCT_DEFINITION_FORMATION('',$,#7849);
#7789=PRODUCT_DEFINITION_FORMATION('',$,#7850);
#7790=PRODUCT_DEFINITION_FORMATION('',$,#7851);
#7791=PRODUCT_DEFINITION_FORMATION('',$,#7852);
#7792=PRODUCT_DEFINITION_FORMATION('',$,#7853);
#7793=PRODUCT_DEFINITION_FORMATION('',$,#7854);
#7794=PRODUCT_DEFINITION_FORMATION('',$,#7855);
#7795=PRODUCT_DEFINITION_FORMATION('',$,#7856);
#7796=PRODUCT_DEFINITION_FORMATION('',$,#7857);
#7797=PRODUCT_DEFINITION_FORMATION('',$,#7858);
#7798=PRODUCT_DEFINITION_FORMATION('',$,#7859);
#7799=PRODUCT_DEFINITION_FORMATION('',$,#7860);
#7800=PRODUCT_DEFINITION_FORMATION('',$,#7861);
#7801=PRODUCT_DEFINITION_FORMATION('',$,#7862);
#7802=PRODUCT_DEFINITION_FORMATION('',$,#7863);
#7803=PRODUCT_DEFINITION_FORMATION('',$,#7864);
#7804=PRODUCT_DEFINITION_FORMATION('',$,#7865);
#7805=PRODUCT_DEFINITION_FORMATION('',$,#7866);
#7806=PRODUCT_DEFINITION_FORMATION('',$,#7867);
#7807=PRODUCT_DEFINITION_FORMATION('',$,#7868);
#7808=PRODUCT_RELATED_PRODUCT_CATEGORY('PAT-057','PAT-057',(#7840));
#7809=PRODUCT_RELATED_PRODUCT_CATEGORY('Side plates and axle',
'Side plates and axle',(#7841));
#7810=PRODUCT_RELATED_PRODUCT_CATEGORY('Side plate','Side plate',(#7842));
#7811=PRODUCT_RELATED_PRODUCT_CATEGORY('Hook bridge','Hook bridge',(#7843));
#7812=PRODUCT_RELATED_PRODUCT_CATEGORY('Eye axle sleeve',
'Eye axle sleeve',(#7844));
#7813=PRODUCT_RELATED_PRODUCT_CATEGORY('Sheave axle','Sheave axle',(#7845));
#7814=PRODUCT_RELATED_PRODUCT_CATEGORY('Axle keeper','Axle keeper',(#7846));
#7815=PRODUCT_RELATED_PRODUCT_CATEGORY('Central inner-race spacer',
'Central inner-race spacer',(#7847));
#7816=PRODUCT_RELATED_PRODUCT_CATEGORY('Hook bushing','Hook bushing',(#7848));
#7817=PRODUCT_RELATED_PRODUCT_CATEGORY('Outer inner-race spacer',
'Outer inner-race spacer',(#7849));
#7818=PRODUCT_RELATED_PRODUCT_CATEGORY('M8x75 cross bolt',
'M8x75 cross bolt',(#7850));
#7819=PRODUCT_RELATED_PRODUCT_CATEGORY('Flat Washer - M8',
'Flat Washer - M8',(#7851));
#7820=PRODUCT_RELATED_PRODUCT_CATEGORY('Hex Nut - M8','Hex Nut - M8',(#7852));
#7821=PRODUCT_RELATED_PRODUCT_CATEGORY('Cap Screw - M8x30',
'Cap Screw - M8x30',(#7853));
#7822=PRODUCT_RELATED_PRODUCT_CATEGORY('Bearing sheave',
'Bearing sheave',(#7854));
#7823=PRODUCT_RELATED_PRODUCT_CATEGORY('Sheave','Sheave',(#7855));
#7824=PRODUCT_RELATED_PRODUCT_CATEGORY('Outer race spacer',
'Outer race spacer',(#7856));
#7825=PRODUCT_RELATED_PRODUCT_CATEGORY(
'Sealed Ball Bearing - 20 x 47 x 14 mm',
'Sealed Ball Bearing - 20 x 47 x 14 mm',(#7857));
#7826=PRODUCT_RELATED_PRODUCT_CATEGORY('Inner ring','Inner ring',(#7858));
#7827=PRODUCT_RELATED_PRODUCT_CATEGORY('Outer ring','Outer ring',(#7859));
#7828=PRODUCT_RELATED_PRODUCT_CATEGORY('Balls','Balls',(#7860));
#7829=PRODUCT_RELATED_PRODUCT_CATEGORY('Cage','Cage',(#7861));
#7830=PRODUCT_RELATED_PRODUCT_CATEGORY('Seals 2RS','Seals 2RS',(#7862));
#7831=PRODUCT_RELATED_PRODUCT_CATEGORY('Sheave cap','Sheave cap',(#7863));
#7832=PRODUCT_RELATED_PRODUCT_CATEGORY('M4x10 Cap Screw',
'M4x10 Cap Screw',(#7864));
#7833=PRODUCT_RELATED_PRODUCT_CATEGORY('Swivelling hook',
'Swivelling hook',(#7865));
#7834=PRODUCT_RELATED_PRODUCT_CATEGORY('Hook','Hook',(#7866));
#7835=PRODUCT_RELATED_PRODUCT_CATEGORY('Swivel thrust washer',
'Swivel thrust washer',(#7867));
#7836=PRODUCT_RELATED_PRODUCT_CATEGORY('M16 hook retaining nut',
'M16 hook retaining nut',(#7868));
#7837=APPLICATION_PROTOCOL_DEFINITION('international standard',
'automotive_design',2009,#7838);
#7838=APPLICATION_CONTEXT(
'Core Data for Automotive Mechanical Design Process');
#7839=PRODUCT_CONTEXT('part definition',#7838,'mechanical');
#7840=PRODUCT('PAT-057','PAT-057',
'PAT-057',(#7839));
#7841=PRODUCT('Side plates and axle','Side plates and axle',
'Side plates and axle',(#7839));
#7842=PRODUCT('Side plate','Side plate','Side plate',(#7839));
#7843=PRODUCT('Hook bridge','Hook bridge','Hook bridge',(#7839));
#7844=PRODUCT('Eye axle sleeve','Eye axle sleeve','Eye axle sleeve',(#7839));
#7845=PRODUCT('Sheave axle','Sheave axle','Sheave axle',(#7839));
#7846=PRODUCT('Axle keeper','Axle keeper','Axle keeper',(#7839));
#7847=PRODUCT('Central inner-race spacer','Central inner-race spacer',
'Central inner-race spacer',(#7839));
#7848=PRODUCT('Hook bushing','Hook bushing','Hook bushing',(#7839));
#7849=PRODUCT('Outer inner-race spacer','Outer inner-race spacer',
'Outer inner-race spacer',(#7839));
#7850=PRODUCT('M8x75 cross bolt','M8x75 cross bolt','M8x75 cross bolt',
(#7839));
#7851=PRODUCT('Flat Washer - M8','Flat Washer - M8','Flat Washer - M8',
(#7839));
#7852=PRODUCT('Hex Nut - M8','Hex Nut - M8','Hex Nut - M8',(#7839));
#7853=PRODUCT('Cap Screw - M8x30','Cap Screw - M8x30',
'Cap Screw - M8x30',(#7839));
#7854=PRODUCT('Bearing sheave','Bearing sheave','Bearing sheave',(#7839));
#7855=PRODUCT('Sheave','Sheave','Sheave',(#7839));
#7856=PRODUCT('Outer race spacer','Outer race spacer',
'Outer race spacer',(#7839));
#7857=PRODUCT('Sealed Ball Bearing - 20 x 47 x 14 mm',
'Sealed Ball Bearing - 20 x 47 x 14 mm',
'Sealed Ball Bearing - 20 x 47 x 14 mm',(#7839));
#7858=PRODUCT('Inner ring','Inner ring','Inner ring',(#7839));
#7859=PRODUCT('Outer ring','Outer ring','Outer ring',(#7839));
#7860=PRODUCT('Balls','Balls','Balls',(#7839));
#7861=PRODUCT('Cage','Cage','Cage',(#7839));
#7862=PRODUCT('Seals 2RS','Seals 2RS','Seals 2RS',(#7839));
#7863=PRODUCT('Sheave cap','Sheave cap','Sheave cap',(#7839));
#7864=PRODUCT('M4x10 Cap Screw','M4x10 Cap Screw','M4x10 Cap Screw',(#7839));
#7865=PRODUCT('Swivelling hook','Swivelling hook','Swivelling hook',(#7839));
#7866=PRODUCT('Hook','Hook','Hook',(#7839));
#7867=PRODUCT('Swivel thrust washer','Swivel thrust washer',
'Swivel thrust washer',(#7839));
#7868=PRODUCT('M16 hook retaining nut','M16 hook retaining nut',
'M16 hook retaining nut',(#7839));
#7869=PRESENTATION_STYLE_ASSIGNMENT((#7874));
#7870=PRESENTATION_STYLE_ASSIGNMENT((#7875));
#7871=PRESENTATION_STYLE_ASSIGNMENT((#7876));
#7872=PRESENTATION_STYLE_ASSIGNMENT((#7877));
#7873=PRESENTATION_STYLE_ASSIGNMENT((#7878));
#7874=SURFACE_STYLE_USAGE(.BOTH.,#7879);
#7875=SURFACE_STYLE_USAGE(.BOTH.,#7880);
#7876=SURFACE_STYLE_USAGE(.BOTH.,#7881);
#7877=SURFACE_STYLE_USAGE(.BOTH.,#7882);
#7878=SURFACE_STYLE_USAGE(.BOTH.,#7883);
#7879=SURFACE_SIDE_STYLE('',(#7884));
#7880=SURFACE_SIDE_STYLE('',(#7885));
#7881=SURFACE_SIDE_STYLE('',(#7886));
#7882=SURFACE_SIDE_STYLE('',(#7887));
#7883=SURFACE_SIDE_STYLE('',(#7888));
#7884=SURFACE_STYLE_FILL_AREA(#7889);
#7885=SURFACE_STYLE_FILL_AREA(#7890);
#7886=SURFACE_STYLE_FILL_AREA(#7891);
#7887=SURFACE_STYLE_FILL_AREA(#7892);
#7888=SURFACE_STYLE_FILL_AREA(#7893);
#7889=FILL_AREA_STYLE('Steel - Satin',(#7894));
#7890=FILL_AREA_STYLE('CAD Library Painted - Engineering blue',(#7895));
#7891=FILL_AREA_STYLE('CAD Library Painted - Steel gray',(#7896));
#7892=FILL_AREA_STYLE('CAD Library Painted - Graphite',(#7897));
#7893=FILL_AREA_STYLE('CAD Library Painted - Off white',(#7898));
#7894=FILL_AREA_STYLE_COLOUR('Steel - Satin',#7899);
#7895=FILL_AREA_STYLE_COLOUR('CAD Library Painted - Engineering blue',#7900);
#7896=FILL_AREA_STYLE_COLOUR('CAD Library Painted - Steel gray',#7901);
#7897=FILL_AREA_STYLE_COLOUR('CAD Library Painted - Graphite',#7902);
#7898=FILL_AREA_STYLE_COLOUR('CAD Library Painted - Off white',#7903);
#7899=COLOUR_RGB('Steel - Satin',0.627450980392157,0.627450980392157,0.627450980392157);
#7900=COLOUR_RGB('CAD Library Painted - Engineering blue',0.12156862745098,
0.356862745098039,0.6);
#7901=COLOUR_RGB('CAD Library Painted - Steel gray',0.592156862745098,0.631372549019608,
0.67843137254902);
#7902=COLOUR_RGB('CAD Library Painted - Graphite',0.0980392156862745,0.109803921568627,
0.125490196078431);
#7903=COLOUR_RGB('CAD Library Painted - Off white',0.909803921568627,0.901960784313726,
0.858823529411765);
#7904=COLOUR_RGB('Dark Blue',0.08,0.2,0.34);
#7905=FILL_AREA_STYLE_COLOUR('',#7904);
#7906=FILL_AREA_STYLE('',(#7905));
#7907=SURFACE_STYLE_FILL_AREA(#7906);
#7908=SURFACE_SIDE_STYLE('',(#7907));
#7909=SURFACE_STYLE_USAGE(.BOTH.,#7908);
#7910=PRESENTATION_STYLE_ASSIGNMENT((#7909));
#7911=COLOUR_RGB('Light Blue',0.38,0.62,0.78);
#7912=FILL_AREA_STYLE_COLOUR('',#7911);
#7913=FILL_AREA_STYLE('',(#7912));
#7914=SURFACE_STYLE_FILL_AREA(#7913);
#7915=SURFACE_SIDE_STYLE('',(#7914));
#7916=SURFACE_STYLE_USAGE(.BOTH.,#7915);
#7917=PRESENTATION_STYLE_ASSIGNMENT((#7916));
#7918=COLOUR_RGB('Sky Blue',0.24,0.69,0.87);
#7919=FILL_AREA_STYLE_COLOUR('',#7918);
#7920=FILL_AREA_STYLE('',(#7919));
#7921=SURFACE_STYLE_FILL_AREA(#7920);
#7922=SURFACE_SIDE_STYLE('',(#7921));
#7923=SURFACE_STYLE_USAGE(.BOTH.,#7922);
#7924=PRESENTATION_STYLE_ASSIGNMENT((#7923));
#7925=COLOUR_RGB('Grey',0.48,0.52,0.57);
#7926=FILL_AREA_STYLE_COLOUR('',#7925);
#7927=FILL_AREA_STYLE('',(#7926));
#7928=SURFACE_STYLE_FILL_AREA(#7927);
#7929=SURFACE_SIDE_STYLE('',(#7928));
#7930=SURFACE_STYLE_USAGE(.BOTH.,#7929);
#7931=PRESENTATION_STYLE_ASSIGNMENT((#7930));
#7932=COLOUR_RGB('Black',0.12,0.14,0.17);
#7933=FILL_AREA_STYLE_COLOUR('',#7932);
#7934=FILL_AREA_STYLE('',(#7933));
#7935=SURFACE_STYLE_FILL_AREA(#7934);
#7936=SURFACE_SIDE_STYLE('',(#7935));
#7937=SURFACE_STYLE_USAGE(.BOTH.,#7936);
#7938=PRESENTATION_STYLE_ASSIGNMENT((#7937));
#7939=COLOUR_RGB('Off White',0.89,0.88,0.83);
#7940=FILL_AREA_STYLE_COLOUR('',#7939);
#7941=FILL_AREA_STYLE('',(#7940));
#7942=SURFACE_STYLE_FILL_AREA(#7941);
#7943=SURFACE_SIDE_STYLE('',(#7942));
#7944=SURFACE_STYLE_USAGE(.BOTH.,#7943);
#7945=PRESENTATION_STYLE_ASSIGNMENT((#7944));
ENDSEC;
END-ISO-10303-21;
